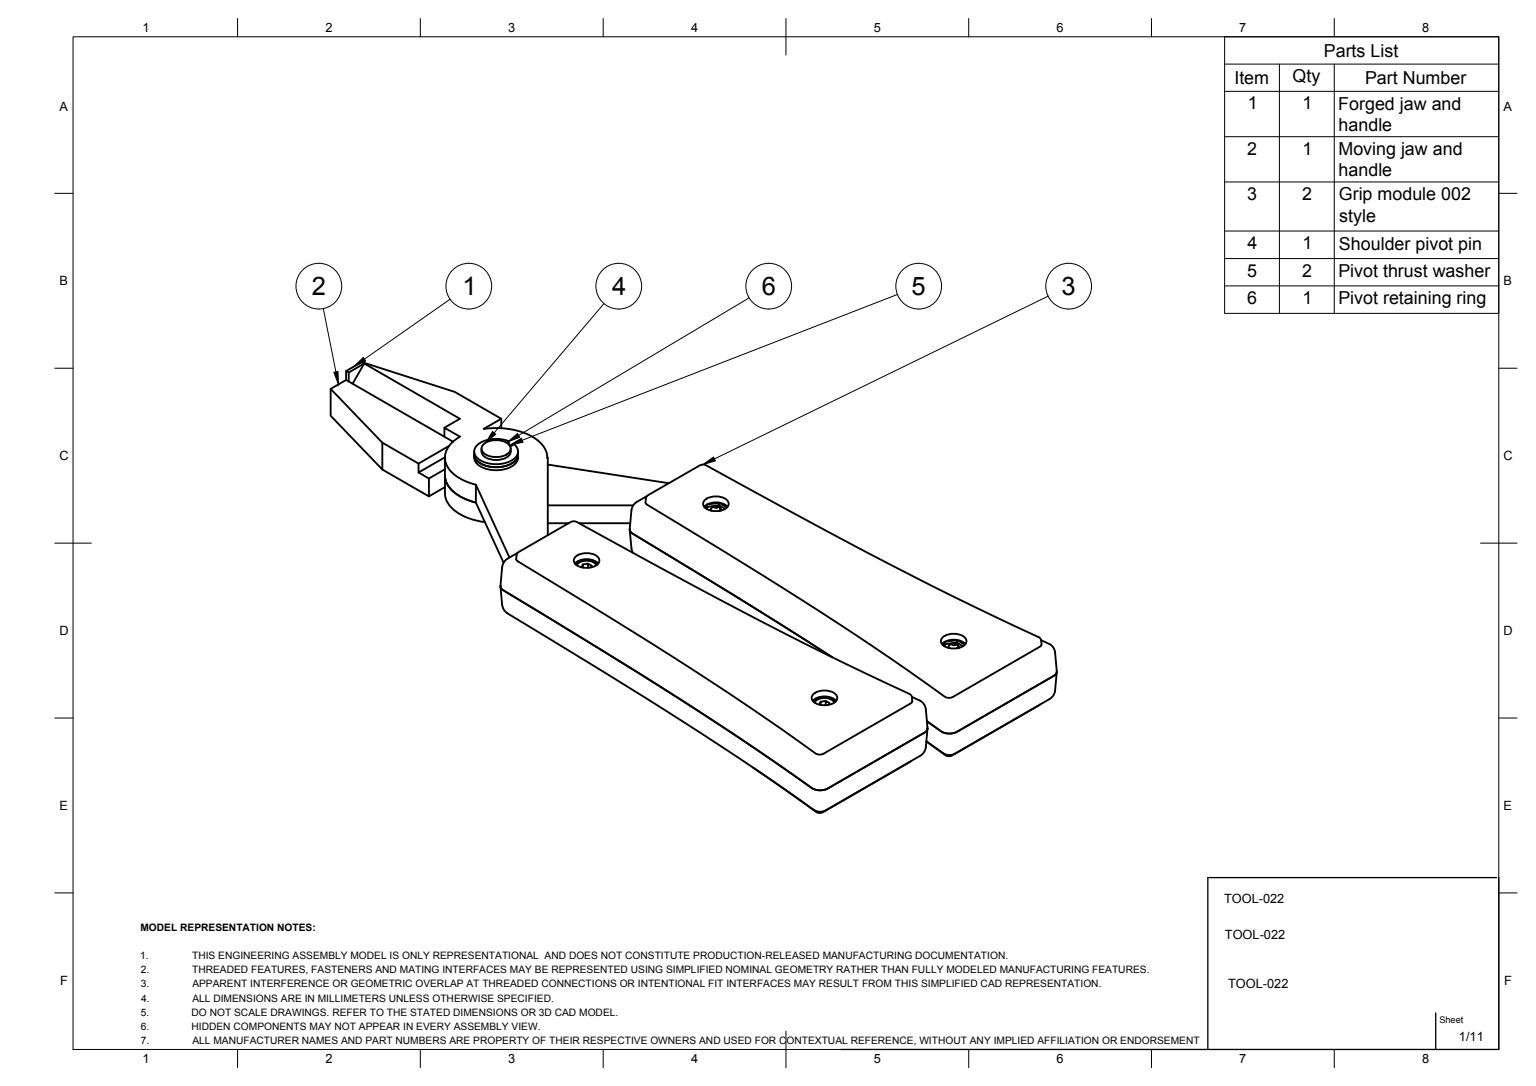
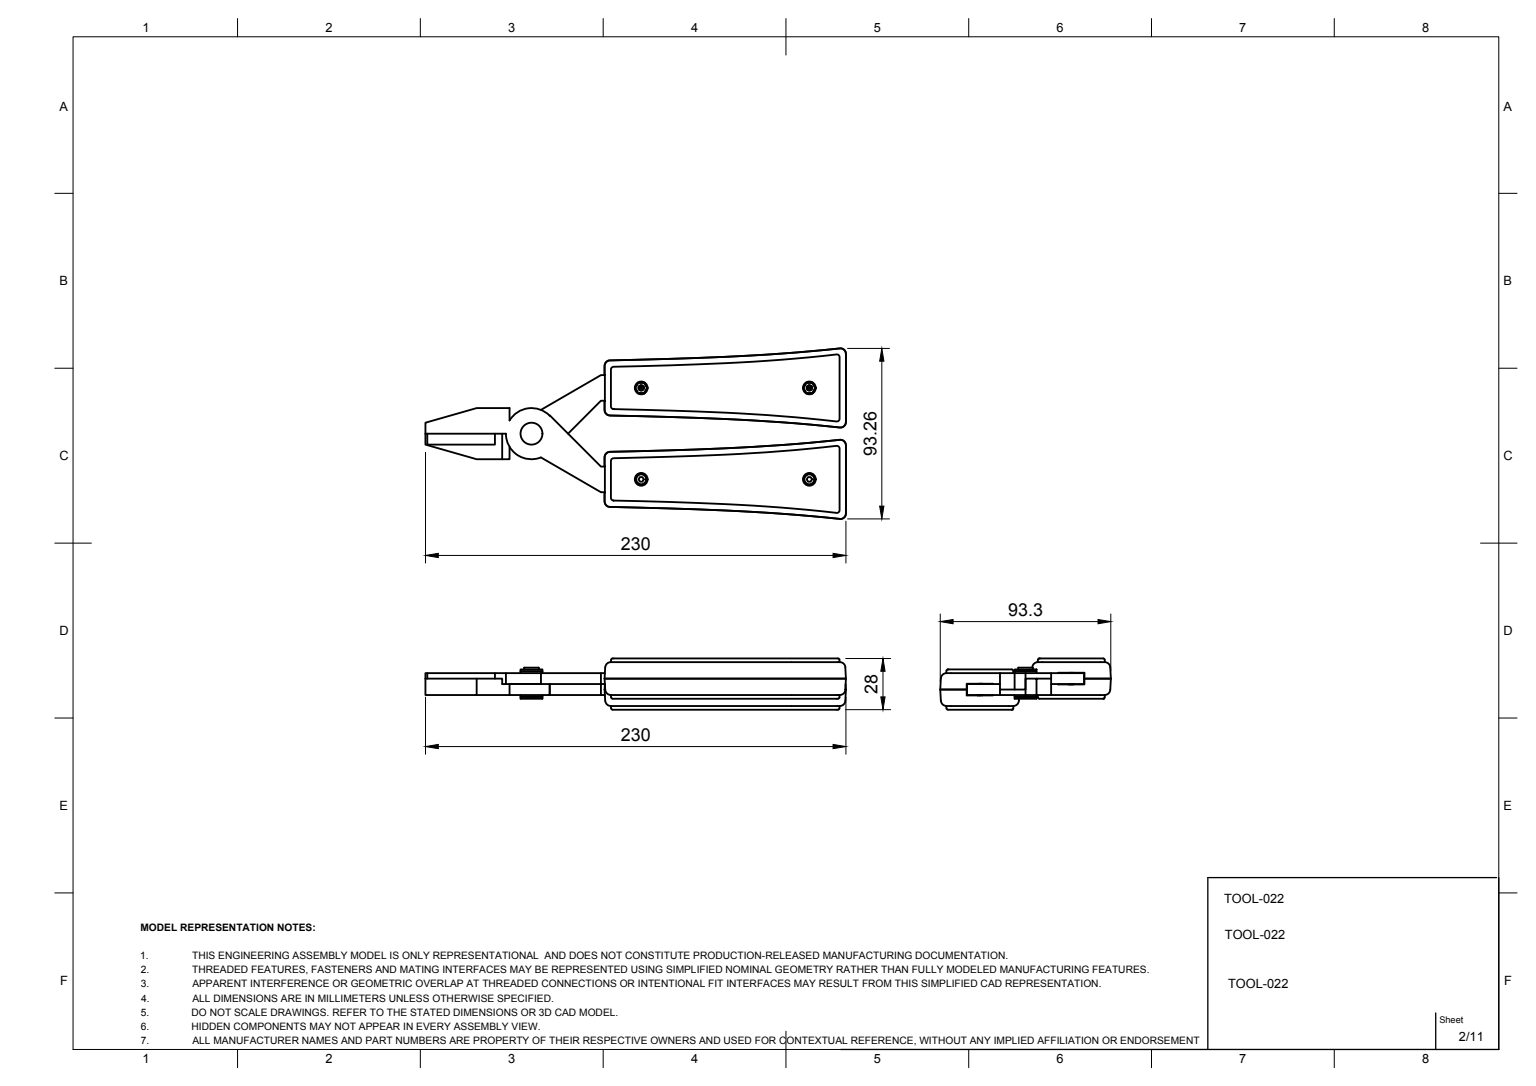
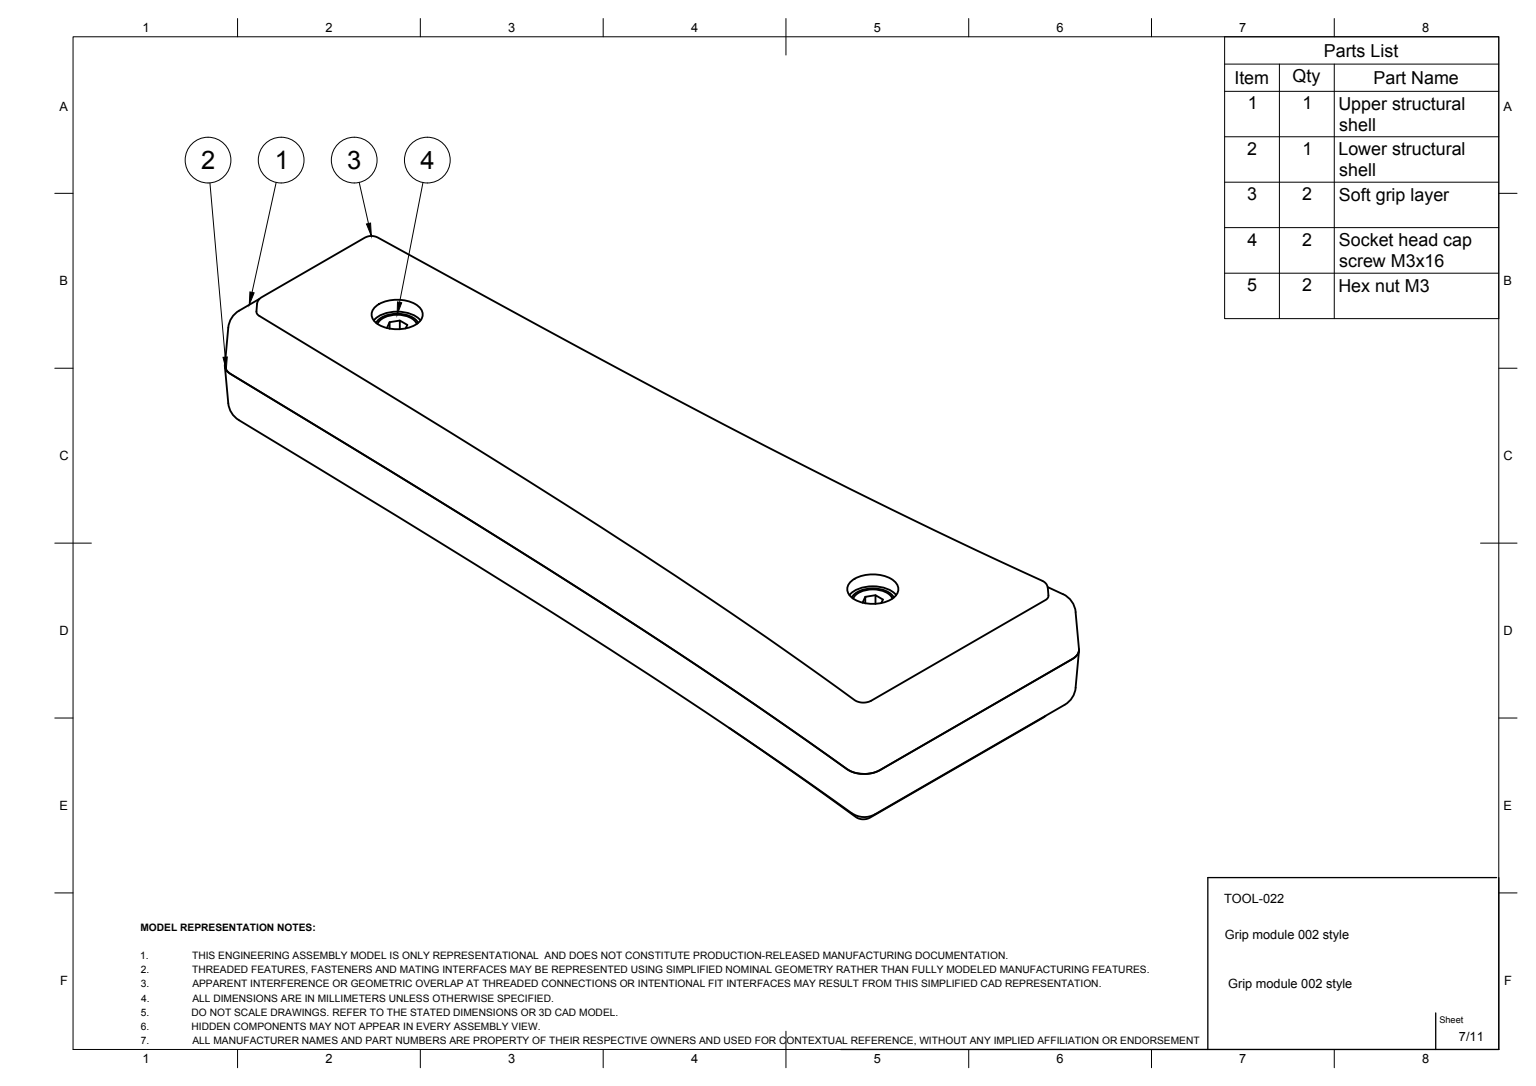
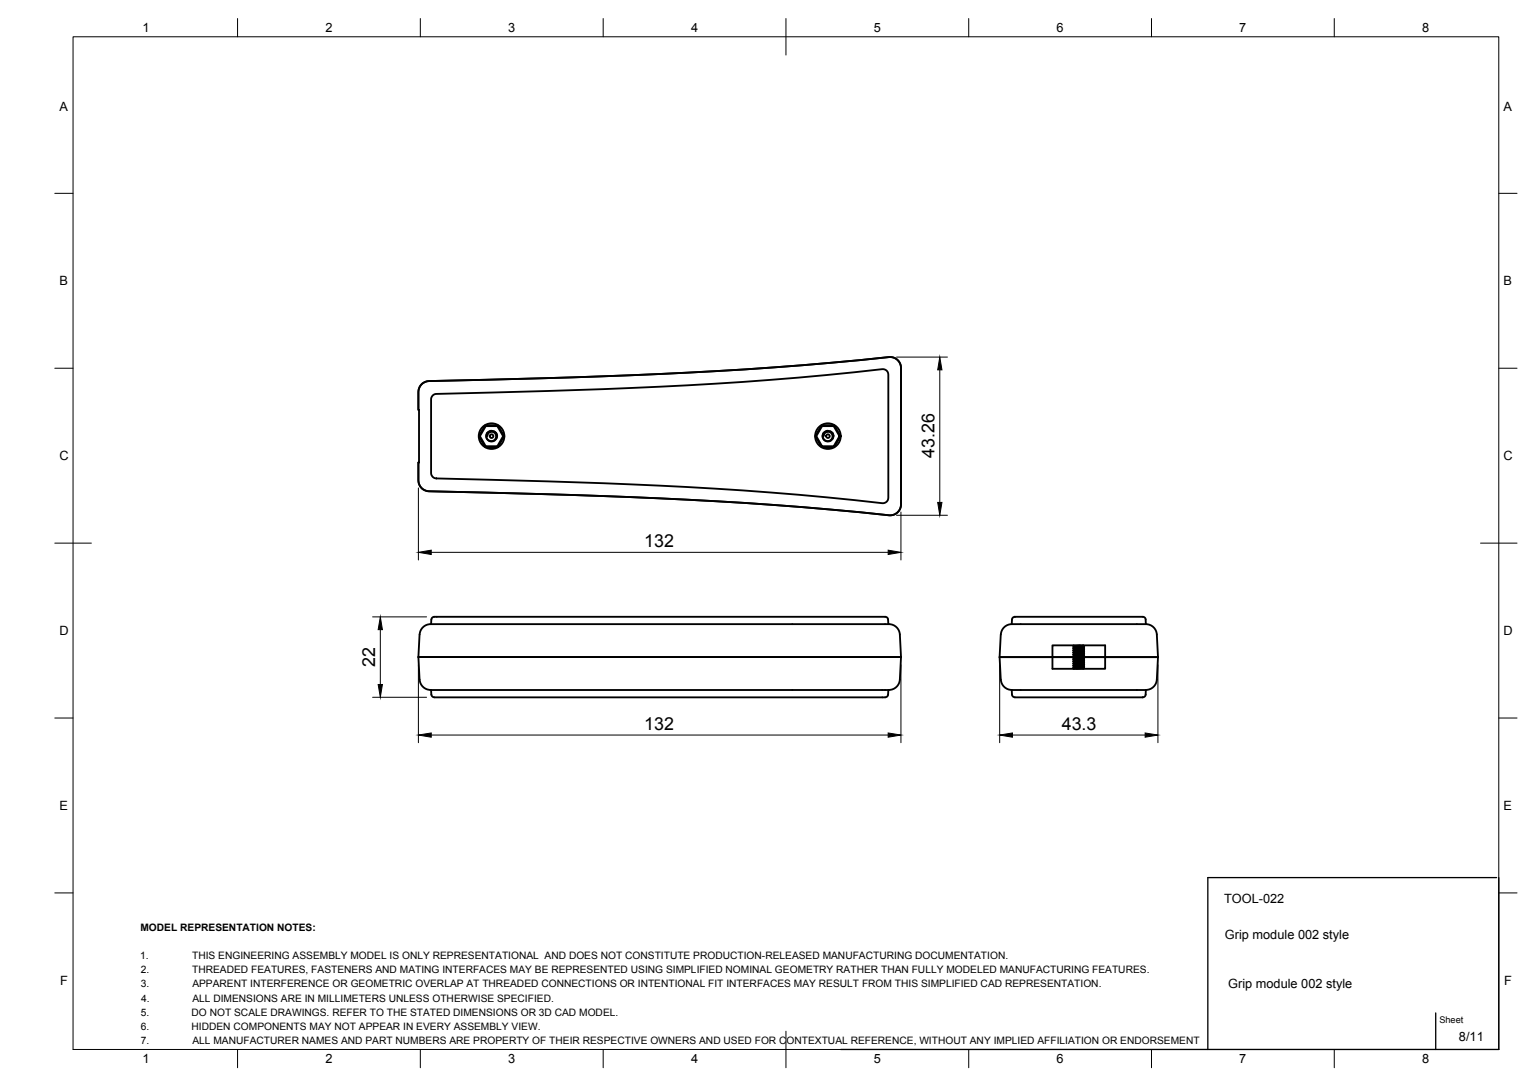
ISO-10303-21;
HEADER;
/* Generated by software containing ST-Developer
 * from STEP Tools, Inc. (www.steptools.com) 
 */

FILE_DESCRIPTION(
/* description */ (''),
/* implementation_level */ '2;1');

FILE_NAME(
/* name */ 'TOOL-022.step',
/* time_stamp */ '2026-11-10T08:27:36-08:00',
/* author */ (''),
/* organization */ (''),
/* preprocessor_version */ 'ST-DEVELOPER v20.2',
/* originating_system */ 'Autodesk Translation Framework v15.17.0.0',
/* authorisation */ '');

FILE_SCHEMA (('AUTOMOTIVE_DESIGN { 1 0 10303 214 3 1 1 }'));
ENDSEC;

DATA;
#10=MECHANICAL_DESIGN_GEOMETRIC_PRESENTATION_REPRESENTATION('',(#566,#567,
#568,#569,#570,#571,#572,#573,#574,#575),#19090);
#11=ITEM_DEFINED_TRANSFORMATION($,$,#7041,#7412);
#12=ITEM_DEFINED_TRANSFORMATION($,$,#7143,#7413);
#13=ITEM_DEFINED_TRANSFORMATION($,$,#7251,#7414);
#14=ITEM_DEFINED_TRANSFORMATION($,$,#7304,#7415);
#15=ITEM_DEFINED_TRANSFORMATION($,$,#7386,#7416);
#16=ITEM_DEFINED_TRANSFORMATION($,$,#7251,#7417);
#17=ITEM_DEFINED_TRANSFORMATION($,$,#7304,#7418);
#18=ITEM_DEFINED_TRANSFORMATION($,$,#7386,#7419);
#19=ITEM_DEFINED_TRANSFORMATION($,$,#6942,#7429);
#20=ITEM_DEFINED_TRANSFORMATION($,$,#6980,#7430);
#21=ITEM_DEFINED_TRANSFORMATION($,$,#7040,#7431);
#22=ITEM_DEFINED_TRANSFORMATION($,$,#7011,#7432);
#23=ITEM_DEFINED_TRANSFORMATION($,$,#7420,#7433);
#24=ITEM_DEFINED_TRANSFORMATION($,$,#7029,#7434);
#25=ITEM_DEFINED_TRANSFORMATION($,$,#7040,#7435);
#26=ITEM_DEFINED_TRANSFORMATION($,$,#7420,#7436);
#27=(
REPRESENTATION_RELATIONSHIP($,$,#19141,#19140)
REPRESENTATION_RELATIONSHIP_WITH_TRANSFORMATION(#11)
SHAPE_REPRESENTATION_RELATIONSHIP()
);
#28=(
REPRESENTATION_RELATIONSHIP($,$,#19142,#19140)
REPRESENTATION_RELATIONSHIP_WITH_TRANSFORMATION(#12)
SHAPE_REPRESENTATION_RELATIONSHIP()
);
#29=(
REPRESENTATION_RELATIONSHIP($,$,#19143,#19140)
REPRESENTATION_RELATIONSHIP_WITH_TRANSFORMATION(#13)
SHAPE_REPRESENTATION_RELATIONSHIP()
);
#30=(
REPRESENTATION_RELATIONSHIP($,$,#19144,#19140)
REPRESENTATION_RELATIONSHIP_WITH_TRANSFORMATION(#14)
SHAPE_REPRESENTATION_RELATIONSHIP()
);
#31=(
REPRESENTATION_RELATIONSHIP($,$,#19145,#19140)
REPRESENTATION_RELATIONSHIP_WITH_TRANSFORMATION(#15)
SHAPE_REPRESENTATION_RELATIONSHIP()
);
#32=(
REPRESENTATION_RELATIONSHIP($,$,#19143,#19140)
REPRESENTATION_RELATIONSHIP_WITH_TRANSFORMATION(#16)
SHAPE_REPRESENTATION_RELATIONSHIP()
);
#33=(
REPRESENTATION_RELATIONSHIP($,$,#19144,#19140)
REPRESENTATION_RELATIONSHIP_WITH_TRANSFORMATION(#17)
SHAPE_REPRESENTATION_RELATIONSHIP()
);
#34=(
REPRESENTATION_RELATIONSHIP($,$,#19145,#19140)
REPRESENTATION_RELATIONSHIP_WITH_TRANSFORMATION(#18)
SHAPE_REPRESENTATION_RELATIONSHIP()
);
#35=(
REPRESENTATION_RELATIONSHIP($,$,#19136,#19135)
REPRESENTATION_RELATIONSHIP_WITH_TRANSFORMATION(#19)
SHAPE_REPRESENTATION_RELATIONSHIP()
);
#36=(
REPRESENTATION_RELATIONSHIP($,$,#19137,#19135)
REPRESENTATION_RELATIONSHIP_WITH_TRANSFORMATION(#20)
SHAPE_REPRESENTATION_RELATIONSHIP()
);
#37=(
REPRESENTATION_RELATIONSHIP($,$,#19140,#19135)
REPRESENTATION_RELATIONSHIP_WITH_TRANSFORMATION(#21)
SHAPE_REPRESENTATION_RELATIONSHIP()
);
#38=(
REPRESENTATION_RELATIONSHIP($,$,#19138,#19135)
REPRESENTATION_RELATIONSHIP_WITH_TRANSFORMATION(#22)
SHAPE_REPRESENTATION_RELATIONSHIP()
);
#39=(
REPRESENTATION_RELATIONSHIP($,$,#19146,#19135)
REPRESENTATION_RELATIONSHIP_WITH_TRANSFORMATION(#23)
SHAPE_REPRESENTATION_RELATIONSHIP()
);
#40=(
REPRESENTATION_RELATIONSHIP($,$,#19139,#19135)
REPRESENTATION_RELATIONSHIP_WITH_TRANSFORMATION(#24)
SHAPE_REPRESENTATION_RELATIONSHIP()
);
#41=(
REPRESENTATION_RELATIONSHIP($,$,#19140,#19135)
REPRESENTATION_RELATIONSHIP_WITH_TRANSFORMATION(#25)
SHAPE_REPRESENTATION_RELATIONSHIP()
);
#42=(
REPRESENTATION_RELATIONSHIP($,$,#19146,#19135)
REPRESENTATION_RELATIONSHIP_WITH_TRANSFORMATION(#26)
SHAPE_REPRESENTATION_RELATIONSHIP()
);
#43=CONTEXT_DEPENDENT_SHAPE_REPRESENTATION(#27,#19118);
#44=CONTEXT_DEPENDENT_SHAPE_REPRESENTATION(#28,#19119);
#45=CONTEXT_DEPENDENT_SHAPE_REPRESENTATION(#29,#19120);
#46=CONTEXT_DEPENDENT_SHAPE_REPRESENTATION(#30,#19121);
#47=CONTEXT_DEPENDENT_SHAPE_REPRESENTATION(#31,#19122);
#48=CONTEXT_DEPENDENT_SHAPE_REPRESENTATION(#32,#19123);
#49=CONTEXT_DEPENDENT_SHAPE_REPRESENTATION(#33,#19124);
#50=CONTEXT_DEPENDENT_SHAPE_REPRESENTATION(#34,#19125);
#51=CONTEXT_DEPENDENT_SHAPE_REPRESENTATION(#35,#19127);
#52=CONTEXT_DEPENDENT_SHAPE_REPRESENTATION(#36,#19128);
#53=CONTEXT_DEPENDENT_SHAPE_REPRESENTATION(#37,#19129);
#54=CONTEXT_DEPENDENT_SHAPE_REPRESENTATION(#38,#19130);
#55=CONTEXT_DEPENDENT_SHAPE_REPRESENTATION(#39,#19131);
#56=CONTEXT_DEPENDENT_SHAPE_REPRESENTATION(#40,#19132);
#57=CONTEXT_DEPENDENT_SHAPE_REPRESENTATION(#41,#19133);
#58=CONTEXT_DEPENDENT_SHAPE_REPRESENTATION(#42,#19134);
#59=NEXT_ASSEMBLY_USAGE_OCCURRENCE('Upper structural shell:1',
'Upper structural shell:1','Upper structural shell:1',#19153,#19154,
'Upper structural shell:1');
#60=NEXT_ASSEMBLY_USAGE_OCCURRENCE('Lower structural shell:1',
'Lower structural shell:1','Lower structural shell:1',#19153,#19155,
'Lower structural shell:1');
#61=NEXT_ASSEMBLY_USAGE_OCCURRENCE('Soft grip layer:1',
'Soft grip layer:1','Soft grip layer:1',#19153,#19156,
'Soft grip layer:1');
#62=NEXT_ASSEMBLY_USAGE_OCCURRENCE('Socket head cap screw M3x16:1',
'Socket head cap screw M3x16:1','Socket head cap screw M3x16:1',#19153,
#19157,'Socket head cap screw M3x16:1');
#63=NEXT_ASSEMBLY_USAGE_OCCURRENCE('Hex nut M3:1','Hex nut M3:1',
'Hex nut M3:1',#19153,#19158,'Hex nut M3:1');
#64=NEXT_ASSEMBLY_USAGE_OCCURRENCE('Soft grip layer:2',
'Soft grip layer:2','Soft grip layer:2',#19153,#19156,
'Soft grip layer:2');
#65=NEXT_ASSEMBLY_USAGE_OCCURRENCE('Socket head cap screw M3x16:2',
'Socket head cap screw M3x16:2','Socket head cap screw M3x16:2',#19153,
#19157,'Socket head cap screw M3x16:2');
#66=NEXT_ASSEMBLY_USAGE_OCCURRENCE('Hex nut M3:2','Hex nut M3:2',
'Hex nut M3:2',#19153,#19158,'Hex nut M3:2');
#67=NEXT_ASSEMBLY_USAGE_OCCURRENCE('Forged jaw and handle:1',
'Forged jaw and handle:1','Forged jaw and handle:1',#19148,#19149,
'Forged jaw and handle:1');
#68=NEXT_ASSEMBLY_USAGE_OCCURRENCE('Moving jaw and handle:1',
'Moving jaw and handle:1','Moving jaw and handle:1',#19148,#19150,
'Moving jaw and handle:1');
#69=NEXT_ASSEMBLY_USAGE_OCCURRENCE('Grip module 002 style:1',
'Grip module 002 style:1','Grip module 002 style:1',#19148,#19153,
'Grip module 002 style:1');
#70=NEXT_ASSEMBLY_USAGE_OCCURRENCE('Shoulder pivot pin:1',
'Shoulder pivot pin:1','Shoulder pivot pin:1',#19148,#19151,
'Shoulder pivot pin:1');
#71=NEXT_ASSEMBLY_USAGE_OCCURRENCE('Pivot thrust washer:1',
'Pivot thrust washer:1','Pivot thrust washer:1',#19148,#19159,
'Pivot thrust washer:1');
#72=NEXT_ASSEMBLY_USAGE_OCCURRENCE('Pivot retaining ring:1',
'Pivot retaining ring:1','Pivot retaining ring:1',#19148,#19152,
'Pivot retaining ring:1');
#73=NEXT_ASSEMBLY_USAGE_OCCURRENCE('Grip module 002 style:2',
'Grip module 002 style:2','Grip module 002 style:2',#19148,#19153,
'Grip module 002 style:2');
#74=NEXT_ASSEMBLY_USAGE_OCCURRENCE('Pivot thrust washer:2',
'Pivot thrust washer:2','Pivot thrust washer:2',#19148,#19159,
'Pivot thrust washer:2');
#75=CONICAL_SURFACE('',#7367,0.1,0.785398163397448);
#76=SPHERICAL_SURFACE('',#7106,0.0999999999999999);
#77=SPHERICAL_SURFACE('',#7109,0.0999999999999997);
#78=SPHERICAL_SURFACE('',#7113,0.0999999999999998);
#79=SPHERICAL_SURFACE('',#7117,0.1);
#80=SPHERICAL_SURFACE('',#7122,0.3);
#81=SPHERICAL_SURFACE('',#7126,0.3);
#82=SPHERICAL_SURFACE('',#7130,0.3);
#83=SPHERICAL_SURFACE('',#7135,0.3);
#84=SPHERICAL_SURFACE('',#7214,0.0999999999999999);
#85=SPHERICAL_SURFACE('',#7217,0.0999999999999997);
#86=SPHERICAL_SURFACE('',#7221,0.0999999999999998);
#87=SPHERICAL_SURFACE('',#7225,0.1);
#88=SPHERICAL_SURFACE('',#7230,0.3);
#89=SPHERICAL_SURFACE('',#7234,0.3);
#90=SPHERICAL_SURFACE('',#7238,0.3);
#91=SPHERICAL_SURFACE('',#7243,0.3);
#92=B_SPLINE_SURFACE_WITH_KNOTS('',3,3,((#10183,#10184,#10185,#10186),(#10187,
#10188,#10189,#10190),(#10191,#10192,#10193,#10194),(#10195,#10196,#10197,
#10198)),.UNSPECIFIED.,.F.,.F.,.F.,(4,4),(4,4),(0.0600191787356395,0.326709122771036),
(0.0105314009467253,0.683686938235975),.UNSPECIFIED.);
#93=B_SPLINE_SURFACE_WITH_KNOTS('',3,3,((#10203,#10204,#10205,#10206),(#10207,
#10208,#10209,#10210),(#10211,#10212,#10213,#10214),(#10215,#10216,#10217,
#10218)),.UNSPECIFIED.,.F.,.F.,.F.,(4,4),(4,4),(0.0251675824878611,0.0470055662028096),
(0.0103663370325175,0.682341693918943),.UNSPECIFIED.);
#94=B_SPLINE_SURFACE_WITH_KNOTS('',3,3,((#10228,#10229,#10230,#10231),(#10232,
#10233,#10234,#10235),(#10236,#10237,#10238,#10239),(#10240,#10241,#10242,
#10243),(#10244,#10245,#10246,#10247)),.UNSPECIFIED.,.F.,.F.,.F.,(4,1,4),
(4,4),(0.,0.571428571428571,1.),(0.796205213256333,4.31873271634551),
 .UNSPECIFIED.);
#95=B_SPLINE_SURFACE_WITH_KNOTS('',3,3,((#10252,#10253,#10254,#10255),(#10256,
#10257,#10258,#10259),(#10260,#10261,#10262,#10263),(#10264,#10265,#10266,
#10267),(#10268,#10269,#10270,#10271)),.UNSPECIFIED.,.F.,.F.,.F.,(4,1,4),
(4,4),(0.,0.571428571428571,1.),(0.335767855111383,0.605460332260614),
 .UNSPECIFIED.);
#96=B_SPLINE_SURFACE_WITH_KNOTS('',3,3,((#10290,#10291,#10292,#10293),(#10294,
#10295,#10296,#10297),(#10298,#10299,#10300,#10301),(#10302,#10303,#10304,
#10305),(#10306,#10307,#10308,#10309)),.UNSPECIFIED.,.F.,.F.,.F.,(4,1,4),
(4,4),(0.,0.571428571428571,1.),(8.8675541747208,12.3900816778099),
 .UNSPECIFIED.);
#97=B_SPLINE_SURFACE_WITH_KNOTS('',3,3,((#10314,#10315,#10316,#10317),(#10318,
#10319,#10320,#10321),(#10322,#10323,#10324,#10325),(#10326,#10327,#10328,
#10329)),.UNSPECIFIED.,.F.,.F.,.F.,(4,4),(4,4),(0.673290877228964,0.939980821264432),
(0.010531400969624,0.683686938235975),.UNSPECIFIED.);
#98=B_SPLINE_SURFACE_WITH_KNOTS('',3,3,((#10330,#10331,#10332,#10333),(#10334,
#10335,#10336,#10337),(#10338,#10339,#10340,#10341),(#10342,#10343,#10344,
#10345)),.UNSPECIFIED.,.F.,.F.,.F.,(4,4),(4,4),(0.952994433797115,0.974832417512139),
(0.0103663370325174,0.682341693895801),.UNSPECIFIED.);
#99=B_SPLINE_SURFACE_WITH_KNOTS('',3,3,((#10429,#10430,#10431,#10432),(#10433,
#10434,#10435,#10436),(#10437,#10438,#10439,#10440),(#10441,#10442,#10443,
#10444)),.UNSPECIFIED.,.F.,.F.,.F.,(4,4),(4,4),(0.341076481775573,0.660379921919131),
(0.0113804342297301,0.684288445414502),.UNSPECIFIED.);
#100=B_SPLINE_SURFACE_WITH_KNOTS('',3,3,((#10449,#10450,#10451,#10452),
(#10453,#10454,#10455,#10456),(#10457,#10458,#10459,#10460),(#10461,#10462,
#10463,#10464),(#10465,#10466,#10467,#10468)),.UNSPECIFIED.,.F.,.F.,.F.,
(4,1,4),(4,4),(0.,0.571428571428571,1.),(4.5128966022766,8.72381854299666),
 .UNSPECIFIED.);
#101=B_SPLINE_SURFACE_WITH_KNOTS('',3,3,((#10478,#10479,#10480,#10481),
(#10482,#10483,#10484,#10485),(#10486,#10487,#10488,#10489),(#10490,#10491,
#10492,#10493),(#10494,#10495,#10496,#10497)),.UNSPECIFIED.,.F.,.F.,.F.,
(4,1,4),(4,4),(0.,0.571428571428571,1.),(4.46246834806959,8.67339028878965),
 .UNSPECIFIED.);
#102=B_SPLINE_SURFACE_WITH_KNOTS('',3,3,((#10502,#10503,#10504,#10505),
(#10506,#10507,#10508,#10509),(#10510,#10511,#10512,#10513),(#10514,#10515,
#10516,#10517)),.UNSPECIFIED.,.F.,.F.,.F.,(4,4),(4,4),(0.33962007808087,
0.658923518224427),(0.0113804342297301,0.68428844541339),.UNSPECIFIED.);
#103=B_SPLINE_SURFACE_WITH_KNOTS('',3,3,((#10589,#10590,#10591,#10592),
(#10593,#10594,#10595,#10596),(#10597,#10598,#10599,#10600),(#10601,#10602,
#10603,#10604)),.UNSPECIFIED.,.F.,.F.,.F.,(4,4),(4,4),(0.67474627241906,
0.91907102854965),(0.0117551961069005,0.684448842095107),.UNSPECIFIED.);
#104=B_SPLINE_SURFACE_WITH_KNOTS('',3,3,((#10609,#10610,#10611,#10612),
(#10613,#10614,#10615,#10616),(#10617,#10618,#10619,#10620),(#10621,#10622,
#10623,#10624),(#10625,#10626,#10627,#10628)),.UNSPECIFIED.,.F.,.F.,.F.,
(4,1,4),(4,4),(0.,0.571428571428571,1.),(8.92068531110742,12.1251256661408),
 .UNSPECIFIED.);
#105=B_SPLINE_SURFACE_WITH_KNOTS('',3,3,((#10629,#10630,#10631,#10632),
(#10633,#10634,#10635,#10636),(#10637,#10638,#10639,#10640),(#10641,#10642,
#10643,#10644),(#10645,#10646,#10647,#10648)),.UNSPECIFIED.,.F.,.F.,.F.,
(4,1,4),(4,4),(0.,0.571428571428571,1.),(1.06116122492545,4.26560157995882),
 .UNSPECIFIED.);
#106=B_SPLINE_SURFACE_WITH_KNOTS('',3,3,((#10653,#10654,#10655,#10656),
(#10657,#10658,#10659,#10660),(#10661,#10662,#10663,#10664),(#10665,#10666,
#10667,#10668)),.UNSPECIFIED.,.F.,.F.,.F.,(4,4),(4,4),(0.0809289714503497,
0.325253727580939),(0.011755196108102,0.684448842095106),.UNSPECIFIED.);
#107=B_SPLINE_SURFACE_WITH_KNOTS('',3,3,((#10743,#10744,#10745,#10746),
(#10747,#10748,#10749,#10750),(#10751,#10752,#10753,#10754),(#10755,#10756,
#10757,#10758)),.UNSPECIFIED.,.F.,.F.,.F.,(4,4),(4,4),(0.932204931312898,
0.977820042778932),(0.0118590921259657,0.68448768567755),.UNSPECIFIED.);
#108=B_SPLINE_SURFACE_WITH_KNOTS('',3,3,((#10768,#10769,#10770,#10771),
(#10772,#10773,#10774,#10775),(#10776,#10777,#10778,#10779),(#10780,#10781,
#10782,#10783),(#10784,#10785,#10786,#10787)),.UNSPECIFIED.,.F.,.F.,.F.,
(4,1,4),(4,4),(0.,0.571428571428571,1.),(12.3228618033436,12.893479658151),
 .UNSPECIFIED.);
#109=B_SPLINE_SURFACE_WITH_KNOTS('',3,3,((#10801,#10802,#10803,#10804),
(#10805,#10806,#10807,#10808),(#10809,#10810,#10811,#10812),(#10813,#10814,
#10815,#10816)),.UNSPECIFIED.,.F.,.F.,.F.,(4,4),(4,4),(0.0221799572210682,
0.0677950686870383),(0.0118590921467069,0.68448768567755),.UNSPECIFIED.);
#110=B_SPLINE_SURFACE_WITH_KNOTS('',3,3,((#10826,#10827,#10828,#10829),
(#10830,#10831,#10832,#10833),(#10834,#10835,#10836,#10837),(#10838,#10839,
#10840,#10841),(#10842,#10843,#10844,#10845)),.UNSPECIFIED.,.F.,.F.,.F.,
(4,1,4),(4,4),(0.,0.571428571428571,1.),(0.29280723291527,0.863425087722636),
 .UNSPECIFIED.);
#111=B_SPLINE_SURFACE_WITH_KNOTS('',3,3,((#10859,#10860,#10861,#10862),
(#10863,#10864,#10865,#10866),(#10867,#10868,#10869,#10870),(#10871,#10872,
#10873,#10874),(#10875,#10876,#10877,#10878)),.UNSPECIFIED.,.F.,.F.,.F.,
(4,1,4),(4,4),(0.,0.571428571428571,1.),(0.00866835330220971,0.617725317592517),
 .UNSPECIFIED.);
#112=B_SPLINE_SURFACE_WITH_KNOTS('',3,3,((#10885,#10886,#10887,#10888),
(#10889,#10890,#10891,#10892),(#10893,#10894,#10895,#10896),(#10897,#10898,
#10899,#10900),(#10901,#10902,#10903,#10904),(#10905,#10906,#10907,#10908)),
 .UNSPECIFIED.,.F.,.F.,.F.,(4,1,1,4),(4,4),(0.,0.285714285714286,0.571428571428571,
1.),(0.00654045782928703,0.615688454110788),.UNSPECIFIED.);
#113=B_SPLINE_SURFACE_WITH_KNOTS('',3,3,((#10913,#10914,#10915,#10916),
(#10917,#10918,#10919,#10920),(#10921,#10922,#10923,#10924),(#10925,#10926,
#10927,#10928),(#10929,#10930,#10931,#10932),(#10933,#10934,#10935,#10936)),
 .UNSPECIFIED.,.F.,.F.,.F.,(4,1,1,4),(4,4),(0.,0.285714285714286,0.571428571428571,
1.),(0.00659363931523289,0.615688454110787),.UNSPECIFIED.);
#114=B_SPLINE_SURFACE_WITH_KNOTS('',3,3,((#10941,#10942,#10943,#10944),
(#10945,#10946,#10947,#10948),(#10949,#10950,#10951,#10952),(#10953,#10954,
#10955,#10956),(#10957,#10958,#10959,#10960)),.UNSPECIFIED.,.F.,.F.,.F.,
(4,1,4),(4,4),(0.,0.571428571428571,1.),(12.5808265588057,12.8505190359549),
 .UNSPECIFIED.);
#115=B_SPLINE_SURFACE_WITH_KNOTS('',3,3,((#10961,#10962,#10963,#10964),
(#10965,#10966,#10967,#10968),(#10969,#10970,#10971,#10972),(#10973,#10974,
#10975,#10976),(#10977,#10978,#10979,#10980)),.UNSPECIFIED.,.F.,.F.,.F.,
(4,1,4),(4,4),(0.,0.571428571428571,1.),(0.00865878607617127,0.617725317592517),
 .UNSPECIFIED.);
#116=B_SPLINE_SURFACE_WITH_KNOTS('',3,3,((#11006,#11007,#11008,#11009),
(#11010,#11011,#11012,#11013),(#11014,#11015,#11016,#11017),(#11018,#11019,
#11020,#11021),(#11022,#11023,#11024,#11025)),.UNSPECIFIED.,.F.,.F.,.F.,
(4,1,4),(4,4),(0.,0.571428571428571,1.),(-0.00615755989250974,0.617725317592517),
 .UNSPECIFIED.);
#117=B_SPLINE_SURFACE_WITH_KNOTS('',3,3,((#11044,#11045,#11046,#11047,#11048),
(#11049,#11050,#11051,#11052,#11053),(#11054,#11055,#11056,#11057,#11058),
(#11059,#11060,#11061,#11062,#11063),(#11064,#11065,#11066,#11067,#11068)),
 .UNSPECIFIED.,.F.,.F.,.F.,(4,1,4),(4,1,4),(0.,0.571428571428571,1.),(0.335767855111383,
5.71764434212835,12.893479658151),.UNSPECIFIED.);
#118=B_SPLINE_SURFACE_WITH_KNOTS('',3,3,((#11079,#11080,#11081,#11082),
(#11083,#11084,#11085,#11086),(#11087,#11088,#11089,#11090),(#11091,#11092,
#11093,#11094),(#11095,#11096,#11097,#11098),(#11099,#11100,#11101,#11102)),
 .UNSPECIFIED.,.F.,.F.,.F.,(4,1,1,4),(4,4),(0.,0.285714285714286,0.571428571428571,
1.),(-0.00844595120920508,0.615688454110788),.UNSPECIFIED.);
#119=B_SPLINE_SURFACE_WITH_KNOTS('',3,3,((#11111,#11112,#11113,#11114),
(#11115,#11116,#11117,#11118),(#11119,#11120,#11121,#11122),(#11123,#11124,
#11125,#11126),(#11127,#11128,#11129,#11130),(#11131,#11132,#11133,#11134)),
 .UNSPECIFIED.,.F.,.F.,.F.,(4,1,1,4),(4,4),(0.,0.285714285714286,0.571428571428571,
1.),(-0.00828643285111643,0.615688454110787),.UNSPECIFIED.);
#120=B_SPLINE_SURFACE_WITH_KNOTS('',3,3,((#11143,#11144,#11145,#11146,#11147),
(#11148,#11149,#11150,#11151,#11152),(#11153,#11154,#11155,#11156,#11157),
(#11158,#11159,#11160,#11161,#11162),(#11163,#11164,#11165,#11166,#11167)),
 .UNSPECIFIED.,.F.,.F.,.F.,(4,1,4),(4,1,4),(0.,0.571428571428571,1.),(0.29280723291527,
7.4686425489379,12.8505190359549),.UNSPECIFIED.);
#121=B_SPLINE_SURFACE_WITH_KNOTS('',3,3,((#11178,#11179,#11180,#11181),
(#11182,#11183,#11184,#11185),(#11186,#11187,#11188,#11189),(#11190,#11191,
#11192,#11193),(#11194,#11195,#11196,#11197)),.UNSPECIFIED.,.F.,.F.,.F.,
(4,1,4),(4,4),(0.,0.571428571428571,1.),(-0.0061862132014275,0.617725317592517),
 .UNSPECIFIED.);
#122=B_SPLINE_SURFACE_WITH_KNOTS('',3,3,((#11206,#11207,#11208,#11209),
(#11210,#11211,#11212,#11213),(#11214,#11215,#11216,#11217),(#11218,#11219,
#11220,#11221)),.UNSPECIFIED.,.F.,.F.,.F.,(4,4),(4,4),(0.025165545222094,
0.977821881680028),(0.,0.68448768567755),.UNSPECIFIED.);
#123=B_SPLINE_SURFACE_WITH_KNOTS('',3,3,((#11224,#11225,#11226,#11227),
(#11228,#11229,#11230,#11231),(#11232,#11233,#11234,#11235),(#11236,#11237,
#11238,#11239)),.UNSPECIFIED.,.F.,.F.,.F.,(4,4),(4,4),(0.0221781183199723,
0.974834454777906),(0.,0.68448768567755),.UNSPECIFIED.);
#124=B_SPLINE_SURFACE_WITH_KNOTS('',3,3,((#12291,#12292,#12293,#12294),
(#12295,#12296,#12297,#12298),(#12299,#12300,#12301,#12302),(#12303,#12304,
#12305,#12306)),.UNSPECIFIED.,.F.,.F.,.F.,(4,4),(4,4),(0.0600191787356395,
0.326709122771036),(0.0105314009467253,0.683686938235975),.UNSPECIFIED.);
#125=B_SPLINE_SURFACE_WITH_KNOTS('',3,3,((#12311,#12312,#12313,#12314),
(#12315,#12316,#12317,#12318),(#12319,#12320,#12321,#12322),(#12323,#12324,
#12325,#12326)),.UNSPECIFIED.,.F.,.F.,.F.,(4,4),(4,4),(0.0251675824878611,
0.0470055662028096),(0.0103663370325175,0.682341693918943),
 .UNSPECIFIED.);
#126=B_SPLINE_SURFACE_WITH_KNOTS('',3,3,((#12336,#12337,#12338,#12339),
(#12340,#12341,#12342,#12343),(#12344,#12345,#12346,#12347),(#12348,#12349,
#12350,#12351),(#12352,#12353,#12354,#12355)),.UNSPECIFIED.,.F.,.F.,.F.,
(4,1,4),(4,4),(0.,0.571428571428571,1.),(0.796205213256333,4.31873271634551),
 .UNSPECIFIED.);
#127=B_SPLINE_SURFACE_WITH_KNOTS('',3,3,((#12360,#12361,#12362,#12363),
(#12364,#12365,#12366,#12367),(#12368,#12369,#12370,#12371),(#12372,#12373,
#12374,#12375),(#12376,#12377,#12378,#12379)),.UNSPECIFIED.,.F.,.F.,.F.,
(4,1,4),(4,4),(0.,0.571428571428571,1.),(0.335767855111383,0.605460332260614),
 .UNSPECIFIED.);
#128=B_SPLINE_SURFACE_WITH_KNOTS('',3,3,((#12398,#12399,#12400,#12401),
(#12402,#12403,#12404,#12405),(#12406,#12407,#12408,#12409),(#12410,#12411,
#12412,#12413),(#12414,#12415,#12416,#12417)),.UNSPECIFIED.,.F.,.F.,.F.,
(4,1,4),(4,4),(0.,0.571428571428571,1.),(8.8675541747208,12.3900816778099),
 .UNSPECIFIED.);
#129=B_SPLINE_SURFACE_WITH_KNOTS('',3,3,((#12422,#12423,#12424,#12425),
(#12426,#12427,#12428,#12429),(#12430,#12431,#12432,#12433),(#12434,#12435,
#12436,#12437)),.UNSPECIFIED.,.F.,.F.,.F.,(4,4),(4,4),(0.673290877228964,
0.939980821264432),(0.010531400969624,0.683686938235975),.UNSPECIFIED.);
#130=B_SPLINE_SURFACE_WITH_KNOTS('',3,3,((#12438,#12439,#12440,#12441),
(#12442,#12443,#12444,#12445),(#12446,#12447,#12448,#12449),(#12450,#12451,
#12452,#12453)),.UNSPECIFIED.,.F.,.F.,.F.,(4,4),(4,4),(0.952994433797115,
0.974832417512139),(0.0103663370325174,0.682341693895801),.UNSPECIFIED.);
#131=B_SPLINE_SURFACE_WITH_KNOTS('',3,3,((#12537,#12538,#12539,#12540),
(#12541,#12542,#12543,#12544),(#12545,#12546,#12547,#12548),(#12549,#12550,
#12551,#12552)),.UNSPECIFIED.,.F.,.F.,.F.,(4,4),(4,4),(0.341076481775573,
0.660379921919131),(0.0113804342297301,0.684288445414502),.UNSPECIFIED.);
#132=B_SPLINE_SURFACE_WITH_KNOTS('',3,3,((#12557,#12558,#12559,#12560),
(#12561,#12562,#12563,#12564),(#12565,#12566,#12567,#12568),(#12569,#12570,
#12571,#12572),(#12573,#12574,#12575,#12576)),.UNSPECIFIED.,.F.,.F.,.F.,
(4,1,4),(4,4),(0.,0.571428571428571,1.),(4.5128966022766,8.72381854299666),
 .UNSPECIFIED.);
#133=B_SPLINE_SURFACE_WITH_KNOTS('',3,3,((#12586,#12587,#12588,#12589),
(#12590,#12591,#12592,#12593),(#12594,#12595,#12596,#12597),(#12598,#12599,
#12600,#12601),(#12602,#12603,#12604,#12605)),.UNSPECIFIED.,.F.,.F.,.F.,
(4,1,4),(4,4),(0.,0.571428571428571,1.),(4.46246834806959,8.67339028878965),
 .UNSPECIFIED.);
#134=B_SPLINE_SURFACE_WITH_KNOTS('',3,3,((#12610,#12611,#12612,#12613),
(#12614,#12615,#12616,#12617),(#12618,#12619,#12620,#12621),(#12622,#12623,
#12624,#12625)),.UNSPECIFIED.,.F.,.F.,.F.,(4,4),(4,4),(0.33962007808087,
0.658923518224427),(0.0113804342297301,0.68428844541339),.UNSPECIFIED.);
#135=B_SPLINE_SURFACE_WITH_KNOTS('',3,3,((#12697,#12698,#12699,#12700),
(#12701,#12702,#12703,#12704),(#12705,#12706,#12707,#12708),(#12709,#12710,
#12711,#12712)),.UNSPECIFIED.,.F.,.F.,.F.,(4,4),(4,4),(0.67474627241906,
0.91907102854965),(0.0117551961069005,0.684448842095107),.UNSPECIFIED.);
#136=B_SPLINE_SURFACE_WITH_KNOTS('',3,3,((#12717,#12718,#12719,#12720),
(#12721,#12722,#12723,#12724),(#12725,#12726,#12727,#12728),(#12729,#12730,
#12731,#12732),(#12733,#12734,#12735,#12736)),.UNSPECIFIED.,.F.,.F.,.F.,
(4,1,4),(4,4),(0.,0.571428571428571,1.),(8.92068531110742,12.1251256661408),
 .UNSPECIFIED.);
#137=B_SPLINE_SURFACE_WITH_KNOTS('',3,3,((#12737,#12738,#12739,#12740),
(#12741,#12742,#12743,#12744),(#12745,#12746,#12747,#12748),(#12749,#12750,
#12751,#12752),(#12753,#12754,#12755,#12756)),.UNSPECIFIED.,.F.,.F.,.F.,
(4,1,4),(4,4),(0.,0.571428571428571,1.),(1.06116122492545,4.26560157995882),
 .UNSPECIFIED.);
#138=B_SPLINE_SURFACE_WITH_KNOTS('',3,3,((#12761,#12762,#12763,#12764),
(#12765,#12766,#12767,#12768),(#12769,#12770,#12771,#12772),(#12773,#12774,
#12775,#12776)),.UNSPECIFIED.,.F.,.F.,.F.,(4,4),(4,4),(0.0809289714503497,
0.325253727580939),(0.011755196108102,0.684448842095106),.UNSPECIFIED.);
#139=B_SPLINE_SURFACE_WITH_KNOTS('',3,3,((#12851,#12852,#12853,#12854),
(#12855,#12856,#12857,#12858),(#12859,#12860,#12861,#12862),(#12863,#12864,
#12865,#12866)),.UNSPECIFIED.,.F.,.F.,.F.,(4,4),(4,4),(0.932204931312898,
0.977820042778932),(0.0118590921259657,0.68448768567755),.UNSPECIFIED.);
#140=B_SPLINE_SURFACE_WITH_KNOTS('',3,3,((#12876,#12877,#12878,#12879),
(#12880,#12881,#12882,#12883),(#12884,#12885,#12886,#12887),(#12888,#12889,
#12890,#12891),(#12892,#12893,#12894,#12895)),.UNSPECIFIED.,.F.,.F.,.F.,
(4,1,4),(4,4),(0.,0.571428571428571,1.),(12.3228618033436,12.893479658151),
 .UNSPECIFIED.);
#141=B_SPLINE_SURFACE_WITH_KNOTS('',3,3,((#12909,#12910,#12911,#12912),
(#12913,#12914,#12915,#12916),(#12917,#12918,#12919,#12920),(#12921,#12922,
#12923,#12924)),.UNSPECIFIED.,.F.,.F.,.F.,(4,4),(4,4),(0.0221799572210682,
0.0677950686870383),(0.0118590921467069,0.68448768567755),.UNSPECIFIED.);
#142=B_SPLINE_SURFACE_WITH_KNOTS('',3,3,((#12934,#12935,#12936,#12937),
(#12938,#12939,#12940,#12941),(#12942,#12943,#12944,#12945),(#12946,#12947,
#12948,#12949),(#12950,#12951,#12952,#12953)),.UNSPECIFIED.,.F.,.F.,.F.,
(4,1,4),(4,4),(0.,0.571428571428571,1.),(0.29280723291527,0.863425087722636),
 .UNSPECIFIED.);
#143=B_SPLINE_SURFACE_WITH_KNOTS('',3,3,((#12967,#12968,#12969,#12970),
(#12971,#12972,#12973,#12974),(#12975,#12976,#12977,#12978),(#12979,#12980,
#12981,#12982),(#12983,#12984,#12985,#12986)),.UNSPECIFIED.,.F.,.F.,.F.,
(4,1,4),(4,4),(0.,0.571428571428571,1.),(0.00866835330220971,0.617725317592517),
 .UNSPECIFIED.);
#144=B_SPLINE_SURFACE_WITH_KNOTS('',3,3,((#12993,#12994,#12995,#12996),
(#12997,#12998,#12999,#13000),(#13001,#13002,#13003,#13004),(#13005,#13006,
#13007,#13008),(#13009,#13010,#13011,#13012),(#13013,#13014,#13015,#13016)),
 .UNSPECIFIED.,.F.,.F.,.F.,(4,1,1,4),(4,4),(0.,0.285714285714286,0.571428571428571,
1.),(0.00654045782928703,0.615688454110788),.UNSPECIFIED.);
#145=B_SPLINE_SURFACE_WITH_KNOTS('',3,3,((#13021,#13022,#13023,#13024),
(#13025,#13026,#13027,#13028),(#13029,#13030,#13031,#13032),(#13033,#13034,
#13035,#13036),(#13037,#13038,#13039,#13040),(#13041,#13042,#13043,#13044)),
 .UNSPECIFIED.,.F.,.F.,.F.,(4,1,1,4),(4,4),(0.,0.285714285714286,0.571428571428571,
1.),(0.00659363931523289,0.615688454110787),.UNSPECIFIED.);
#146=B_SPLINE_SURFACE_WITH_KNOTS('',3,3,((#13049,#13050,#13051,#13052),
(#13053,#13054,#13055,#13056),(#13057,#13058,#13059,#13060),(#13061,#13062,
#13063,#13064),(#13065,#13066,#13067,#13068)),.UNSPECIFIED.,.F.,.F.,.F.,
(4,1,4),(4,4),(0.,0.571428571428571,1.),(12.5808265588057,12.8505190359549),
 .UNSPECIFIED.);
#147=B_SPLINE_SURFACE_WITH_KNOTS('',3,3,((#13069,#13070,#13071,#13072),
(#13073,#13074,#13075,#13076),(#13077,#13078,#13079,#13080),(#13081,#13082,
#13083,#13084),(#13085,#13086,#13087,#13088)),.UNSPECIFIED.,.F.,.F.,.F.,
(4,1,4),(4,4),(0.,0.571428571428571,1.),(0.00865878607617127,0.617725317592517),
 .UNSPECIFIED.);
#148=B_SPLINE_SURFACE_WITH_KNOTS('',3,3,((#13114,#13115,#13116,#13117),
(#13118,#13119,#13120,#13121),(#13122,#13123,#13124,#13125),(#13126,#13127,
#13128,#13129),(#13130,#13131,#13132,#13133)),.UNSPECIFIED.,.F.,.F.,.F.,
(4,1,4),(4,4),(0.,0.571428571428571,1.),(-0.00615755989250974,0.617725317592517),
 .UNSPECIFIED.);
#149=B_SPLINE_SURFACE_WITH_KNOTS('',3,3,((#13152,#13153,#13154,#13155,#13156),
(#13157,#13158,#13159,#13160,#13161),(#13162,#13163,#13164,#13165,#13166),
(#13167,#13168,#13169,#13170,#13171),(#13172,#13173,#13174,#13175,#13176)),
 .UNSPECIFIED.,.F.,.F.,.F.,(4,1,4),(4,1,4),(0.,0.571428571428571,1.),(0.335767855111383,
5.71764434212835,12.893479658151),.UNSPECIFIED.);
#150=B_SPLINE_SURFACE_WITH_KNOTS('',3,3,((#13187,#13188,#13189,#13190),
(#13191,#13192,#13193,#13194),(#13195,#13196,#13197,#13198),(#13199,#13200,
#13201,#13202),(#13203,#13204,#13205,#13206),(#13207,#13208,#13209,#13210)),
 .UNSPECIFIED.,.F.,.F.,.F.,(4,1,1,4),(4,4),(0.,0.285714285714286,0.571428571428571,
1.),(-0.00844595120920508,0.615688454110788),.UNSPECIFIED.);
#151=B_SPLINE_SURFACE_WITH_KNOTS('',3,3,((#13219,#13220,#13221,#13222),
(#13223,#13224,#13225,#13226),(#13227,#13228,#13229,#13230),(#13231,#13232,
#13233,#13234),(#13235,#13236,#13237,#13238),(#13239,#13240,#13241,#13242)),
 .UNSPECIFIED.,.F.,.F.,.F.,(4,1,1,4),(4,4),(0.,0.285714285714286,0.571428571428571,
1.),(-0.00828643285111643,0.615688454110787),.UNSPECIFIED.);
#152=B_SPLINE_SURFACE_WITH_KNOTS('',3,3,((#13251,#13252,#13253,#13254,#13255),
(#13256,#13257,#13258,#13259,#13260),(#13261,#13262,#13263,#13264,#13265),
(#13266,#13267,#13268,#13269,#13270),(#13271,#13272,#13273,#13274,#13275)),
 .UNSPECIFIED.,.F.,.F.,.F.,(4,1,4),(4,1,4),(0.,0.571428571428571,1.),(0.29280723291527,
7.4686425489379,12.8505190359549),.UNSPECIFIED.);
#153=B_SPLINE_SURFACE_WITH_KNOTS('',3,3,((#13286,#13287,#13288,#13289),
(#13290,#13291,#13292,#13293),(#13294,#13295,#13296,#13297),(#13298,#13299,
#13300,#13301),(#13302,#13303,#13304,#13305)),.UNSPECIFIED.,.F.,.F.,.F.,
(4,1,4),(4,4),(0.,0.571428571428571,1.),(-0.0061862132014275,0.617725317592517),
 .UNSPECIFIED.);
#154=B_SPLINE_SURFACE_WITH_KNOTS('',3,3,((#13314,#13315,#13316,#13317),
(#13318,#13319,#13320,#13321),(#13322,#13323,#13324,#13325),(#13326,#13327,
#13328,#13329)),.UNSPECIFIED.,.F.,.F.,.F.,(4,4),(4,4),(0.025165545222094,
0.977821881680028),(0.,0.68448768567755),.UNSPECIFIED.);
#155=B_SPLINE_SURFACE_WITH_KNOTS('',3,3,((#13332,#13333,#13334,#13335),
(#13336,#13337,#13338,#13339),(#13340,#13341,#13342,#13343),(#13344,#13345,
#13346,#13347)),.UNSPECIFIED.,.F.,.F.,.F.,(4,4),(4,4),(0.0221781183199723,
0.974834454777906),(0.,0.68448768567755),.UNSPECIFIED.);
#156=B_SPLINE_SURFACE_WITH_KNOTS('',3,3,((#13418,#13419,#13420,#13421,#13422),
(#13423,#13424,#13425,#13426,#13427),(#13428,#13429,#13430,#13431,#13432),
(#13433,#13434,#13435,#13436,#13437),(#13438,#13439,#13440,#13441,#13442)),
 .UNSPECIFIED.,.F.,.F.,.F.,(4,1,4),(4,1,4),(0.,0.571428571428571,1.),(0.,
0.0505788685273923,0.118017359897249),.UNSPECIFIED.);
#157=B_SPLINE_SURFACE_WITH_KNOTS('',3,3,((#13465,#13466,#13467,#13468,#13469),
(#13470,#13471,#13472,#13473,#13474),(#13475,#13476,#13477,#13478,#13479),
(#13480,#13481,#13482,#13483,#13484),(#13485,#13486,#13487,#13488,#13489)),
 .UNSPECIFIED.,.F.,.F.,.F.,(4,1,4),(4,1,4),(0.,0.571428571428571,1.),(0.,
0.0505788685278266,0.118017359898262),.UNSPECIFIED.);
#158=B_SPLINE_SURFACE_WITH_KNOTS('',3,3,((#13503,#13504,#13505,#13506,#13507),
(#13508,#13509,#13510,#13511,#13512),(#13513,#13514,#13515,#13516,#13517),
(#13518,#13519,#13520,#13521,#13522),(#13523,#13524,#13525,#13526,#13527)),
 .UNSPECIFIED.,.F.,.F.,.F.,(4,1,4),(4,1,4),(0.,0.571428571428571,1.),(0.,
5.23288834931112,12.2100728150593),.UNSPECIFIED.);
#159=B_SPLINE_SURFACE_WITH_KNOTS('',3,3,((#13541,#13542,#13543,#13544,#13545),
(#13546,#13547,#13548,#13549,#13550),(#13551,#13552,#13553,#13554,#13555),
(#13556,#13557,#13558,#13559,#13560),(#13561,#13562,#13563,#13564,#13565)),
 .UNSPECIFIED.,.F.,.F.,.F.,(4,1,4),(4,1,4),(0.,0.571428571428571,1.),(1.97133828064127E-11,
0.0463413823988794,0.108129892237767),.UNSPECIFIED.);
#160=B_SPLINE_SURFACE_WITH_KNOTS('',3,3,((#13585,#13586,#13587,#13588,#13589),
(#13590,#13591,#13592,#13593,#13594),(#13595,#13596,#13597,#13598,#13599),
(#13600,#13601,#13602,#13603,#13604),(#13605,#13606,#13607,#13608,#13609)),
 .UNSPECIFIED.,.F.,.F.,.F.,(4,1,4),(4,1,4),(0.,0.571428571428571,1.),(0.,
0.0463413823743492,0.108129892206815),.UNSPECIFIED.);
#161=B_SPLINE_SURFACE_WITH_KNOTS('',3,3,((#13623,#13624,#13625,#13626,#13627),
(#13628,#13629,#13630,#13631,#13632),(#13633,#13634,#13635,#13636,#13637),
(#13638,#13639,#13640,#13641,#13642),(#13643,#13644,#13645,#13646,#13647)),
 .UNSPECIFIED.,.F.,.F.,.F.,(4,1,4),(4,1,4),(0.,0.571428571428571,1.),(6.51086303075479E-13,
6.97718480957529,12.2100734167563),.UNSPECIFIED.);
#162=B_SPLINE_SURFACE_WITH_KNOTS('',3,3,((#13670,#13671,#13672,#13673),
(#13674,#13675,#13676,#13677),(#13678,#13679,#13680,#13681),(#13682,#13683,
#13684,#13685),(#13686,#13687,#13688,#13689)),.UNSPECIFIED.,.F.,.F.,.F.,
(4,1,4),(4,4),(0.,0.571428571428571,1.),(-0.00308447593286339,0.124708996845866),
 .UNSPECIFIED.);
#163=B_SPLINE_SURFACE_WITH_KNOTS('',3,3,((#13723,#13724,#13725,#13726),
(#13727,#13728,#13729,#13730),(#13731,#13732,#13733,#13734),(#13735,#13736,
#13737,#13738)),.UNSPECIFIED.,.F.,.F.,.F.,(4,4),(4,4),(0.0116899650356219,
0.986620910196183),(0.,0.621418053543664),.UNSPECIFIED.);
#164=B_SPLINE_SURFACE_WITH_KNOTS('',3,3,((#13748,#13749,#13750,#13751),
(#13752,#13753,#13754,#13755),(#13756,#13757,#13758,#13759),(#13760,#13761,
#13762,#13763),(#13764,#13765,#13766,#13767),(#13768,#13769,#13770,#13771)),
 .UNSPECIFIED.,.F.,.F.,.F.,(4,1,1,4),(4,4),(0.,0.285714285714286,0.571428571428571,
1.),(-0.00421817271916687,0.124025126494243),.UNSPECIFIED.);
#165=B_SPLINE_SURFACE_WITH_KNOTS('',3,3,((#13819,#13820,#13821,#13822),
(#13823,#13824,#13825,#13826),(#13827,#13828,#13829,#13830),(#13831,#13832,
#13833,#13834),(#13835,#13836,#13837,#13838)),.UNSPECIFIED.,.F.,.F.,.F.,
(4,1,4),(4,4),(0.,0.571428571428571,1.),(-0.00306862226109154,0.124708996851356),
 .UNSPECIFIED.);
#166=B_SPLINE_SURFACE_WITH_KNOTS('',3,3,((#13872,#13873,#13874,#13875),
(#13876,#13877,#13878,#13879),(#13880,#13881,#13882,#13883),(#13884,#13885,
#13886,#13887),(#13888,#13889,#13890,#13891),(#13892,#13893,#13894,#13895)),
 .UNSPECIFIED.,.F.,.F.,.F.,(4,1,1,4),(4,4),(0.,0.285714285714286,0.571428571428571,
1.),(-0.00430078538920315,0.12402512649425),.UNSPECIFIED.);
#167=B_SPLINE_SURFACE_WITH_KNOTS('',3,3,((#13940,#13941,#13942,#13943),
(#13944,#13945,#13946,#13947),(#13948,#13949,#13950,#13951),(#13952,#13953,
#13954,#13955)),.UNSPECIFIED.,.F.,.F.,.F.,(4,4),(4,4),(0.0133790898038168,
0.988310034964378),(0.,0.621418053491537),.UNSPECIFIED.);
#168=B_SPLINE_SURFACE_WITH_KNOTS('',3,3,((#16338,#16339,#16340,#16341,#16342,
#16343,#16344,#16345,#16346,#16347,#16348,#16349,#16350,#16351,#16352,#16353,
#16354,#16355,#16356,#16357,#16358,#16359,#16360,#16361,#16362,#16363,#16364,
#16365,#16366,#16367,#16368,#16369,#16370,#16371,#16372,#16373,#16374,#16375,
#16376,#16377,#16378,#16379,#16380,#16381,#16382,#16383,#16384,#16385,#16386,
#16387,#16388,#16389,#16390,#16391,#16392,#16393,#16394,#16395,#16396,#16397,
#16398,#16399,#16400,#16401,#16402,#16403,#16404,#16405,#16406,#16407,#16408,
#16409,#16410,#16411,#16412,#16413,#16414,#16415,#16416,#16417,#16418,#16419,
#16420,#16421,#16422,#16423,#16424,#16425,#16426,#16427,#16428,#16429,#16430,
#16431,#16432,#16433,#16434,#16435,#16436,#16437,#16438,#16439,#16440,#16441,
#16442,#16443,#16444,#16445,#16446,#16447,#16448,#16449,#16450,#16451,#16452,
#16453,#16454,#16455,#16456,#16457,#16458,#16459,#16460,#16461,#16462,#16463,
#16464,#16465,#16466,#16467,#16468,#16469,#16470,#16471,#16472,#16473,#16474,
#16475,#16476,#16477,#16478,#16479,#16480,#16481,#16482,#16483,#16484,#16485,
#16486,#16487,#16488,#16489,#16490,#16491,#16492,#16493,#16494,#16495,#16496,
#16497,#16498,#16499,#16500,#16501,#16502,#16503,#16504,#16505,#16506,#16507,
#16508,#16509,#16510,#16511,#16512,#16513,#16514,#16515,#16516,#16517,#16518,
#16519,#16520,#16521,#16522,#16523,#16524,#16525,#16526,#16527,#16528,#16529,
#16530,#16531,#16532,#16533),(#16534,#16535,#16536,#16537,#16538,#16539,
#16540,#16541,#16542,#16543,#16544,#16545,#16546,#16547,#16548,#16549,#16550,
#16551,#16552,#16553,#16554,#16555,#16556,#16557,#16558,#16559,#16560,#16561,
#16562,#16563,#16564,#16565,#16566,#16567,#16568,#16569,#16570,#16571,#16572,
#16573,#16574,#16575,#16576,#16577,#16578,#16579,#16580,#16581,#16582,#16583,
#16584,#16585,#16586,#16587,#16588,#16589,#16590,#16591,#16592,#16593,#16594,
#16595,#16596,#16597,#16598,#16599,#16600,#16601,#16602,#16603,#16604,#16605,
#16606,#16607,#16608,#16609,#16610,#16611,#16612,#16613,#16614,#16615,#16616,
#16617,#16618,#16619,#16620,#16621,#16622,#16623,#16624,#16625,#16626,#16627,
#16628,#16629,#16630,#16631,#16632,#16633,#16634,#16635,#16636,#16637,#16638,
#16639,#16640,#16641,#16642,#16643,#16644,#16645,#16646,#16647,#16648,#16649,
#16650,#16651,#16652,#16653,#16654,#16655,#16656,#16657,#16658,#16659,#16660,
#16661,#16662,#16663,#16664,#16665,#16666,#16667,#16668,#16669,#16670,#16671,
#16672,#16673,#16674,#16675,#16676,#16677,#16678,#16679,#16680,#16681,#16682,
#16683,#16684,#16685,#16686,#16687,#16688,#16689,#16690,#16691,#16692,#16693,
#16694,#16695,#16696,#16697,#16698,#16699,#16700,#16701,#16702,#16703,#16704,
#16705,#16706,#16707,#16708,#16709,#16710,#16711,#16712,#16713,#16714,#16715,
#16716,#16717,#16718,#16719,#16720,#16721,#16722,#16723,#16724,#16725,#16726,
#16727,#16728,#16729),(#16730,#16731,#16732,#16733,#16734,#16735,#16736,
#16737,#16738,#16739,#16740,#16741,#16742,#16743,#16744,#16745,#16746,#16747,
#16748,#16749,#16750,#16751,#16752,#16753,#16754,#16755,#16756,#16757,#16758,
#16759,#16760,#16761,#16762,#16763,#16764,#16765,#16766,#16767,#16768,#16769,
#16770,#16771,#16772,#16773,#16774,#16775,#16776,#16777,#16778,#16779,#16780,
#16781,#16782,#16783,#16784,#16785,#16786,#16787,#16788,#16789,#16790,#16791,
#16792,#16793,#16794,#16795,#16796,#16797,#16798,#16799,#16800,#16801,#16802,
#16803,#16804,#16805,#16806,#16807,#16808,#16809,#16810,#16811,#16812,#16813,
#16814,#16815,#16816,#16817,#16818,#16819,#16820,#16821,#16822,#16823,#16824,
#16825,#16826,#16827,#16828,#16829,#16830,#16831,#16832,#16833,#16834,#16835,
#16836,#16837,#16838,#16839,#16840,#16841,#16842,#16843,#16844,#16845,#16846,
#16847,#16848,#16849,#16850,#16851,#16852,#16853,#16854,#16855,#16856,#16857,
#16858,#16859,#16860,#16861,#16862,#16863,#16864,#16865,#16866,#16867,#16868,
#16869,#16870,#16871,#16872,#16873,#16874,#16875,#16876,#16877,#16878,#16879,
#16880,#16881,#16882,#16883,#16884,#16885,#16886,#16887,#16888,#16889,#16890,
#16891,#16892,#16893,#16894,#16895,#16896,#16897,#16898,#16899,#16900,#16901,
#16902,#16903,#16904,#16905,#16906,#16907,#16908,#16909,#16910,#16911,#16912,
#16913,#16914,#16915,#16916,#16917,#16918,#16919,#16920,#16921,#16922,#16923,
#16924,#16925),(#16926,#16927,#16928,#16929,#16930,#16931,#16932,#16933,
#16934,#16935,#16936,#16937,#16938,#16939,#16940,#16941,#16942,#16943,#16944,
#16945,#16946,#16947,#16948,#16949,#16950,#16951,#16952,#16953,#16954,#16955,
#16956,#16957,#16958,#16959,#16960,#16961,#16962,#16963,#16964,#16965,#16966,
#16967,#16968,#16969,#16970,#16971,#16972,#16973,#16974,#16975,#16976,#16977,
#16978,#16979,#16980,#16981,#16982,#16983,#16984,#16985,#16986,#16987,#16988,
#16989,#16990,#16991,#16992,#16993,#16994,#16995,#16996,#16997,#16998,#16999,
#17000,#17001,#17002,#17003,#17004,#17005,#17006,#17007,#17008,#17009,#17010,
#17011,#17012,#17013,#17014,#17015,#17016,#17017,#17018,#17019,#17020,#17021,
#17022,#17023,#17024,#17025,#17026,#17027,#17028,#17029,#17030,#17031,#17032,
#17033,#17034,#17035,#17036,#17037,#17038,#17039,#17040,#17041,#17042,#17043,
#17044,#17045,#17046,#17047,#17048,#17049,#17050,#17051,#17052,#17053,#17054,
#17055,#17056,#17057,#17058,#17059,#17060,#17061,#17062,#17063,#17064,#17065,
#17066,#17067,#17068,#17069,#17070,#17071,#17072,#17073,#17074,#17075,#17076,
#17077,#17078,#17079,#17080,#17081,#17082,#17083,#17084,#17085,#17086,#17087,
#17088,#17089,#17090,#17091,#17092,#17093,#17094,#17095,#17096,#17097,#17098,
#17099,#17100,#17101,#17102,#17103,#17104,#17105,#17106,#17107,#17108,#17109,
#17110,#17111,#17112,#17113,#17114,#17115,#17116,#17117,#17118,#17119,#17120,
#17121)),.UNSPECIFIED.,.F.,.F.,.F.,(4,4),(4,1,1,1,1,1,1,1,1,1,1,1,1,1,1,
1,1,1,1,1,1,1,1,1,1,1,1,1,1,1,1,1,1,1,1,1,1,1,1,1,1,1,1,1,1,1,1,1,1,1,1,
1,1,1,1,1,1,1,1,1,1,1,1,1,1,1,1,1,1,1,1,1,1,1,1,1,1,1,1,1,1,1,1,1,1,1,1,
1,1,1,1,1,1,1,1,1,1,1,1,1,1,1,1,1,1,1,1,1,1,1,1,1,1,1,1,1,1,1,1,1,1,1,1,
1,1,1,1,1,1,1,1,1,1,1,1,1,1,1,1,1,1,1,1,1,1,1,1,1,1,1,1,1,1,1,1,1,1,1,1,
1,1,1,1,1,1,1,1,1,1,1,1,1,1,1,1,1,1,1,1,1,1,1,1,1,1,1,1,1,1,1,1,1,1,4),
(0.,0.0329955678841871),(11.6159397475006,12.61358260836,13.6112254692194,
14.6088683300789,15.6065111909383,16.6041540517977,17.6017969126571,18.5994397735165,
19.5970826343759,20.5947254952353,21.5923683560947,22.5900112169541,23.5876540778135,
24.5852969386729,25.5829397995323,26.5805826603917,27.5782255212511,28.5758683821105,
29.5735112429699,30.5711541038294,31.5687969646888,32.5664398255482,33.5640826864076,
34.561725547267,35.5593684081264,36.5570112689858,37.5546541298452,38.5522969907046,
39.549939851564,40.5475827124234,41.5452255732828,42.5428684341422,43.5405112950016,
44.538154155861,45.5357970167204,46.5334398775799,47.5310827384393,48.5287255992987,
49.5263684601581,50.5240113210175,51.5216541818769,52.5192970427363,53.5169399035957,
54.5145827644551,55.5122256253145,56.5098684861739,57.5075113470333,58.5051542078927,
59.5027970687521,60.5004399296115,61.4980827904709,62.4957256513303,63.4933685121897,
64.4910113730492,65.4886542339086,66.486297094768,67.4839399556274,68.4815828164868,
69.4792256773462,70.4768685382056,71.474511399065,72.4721542599244,73.4697971207838,
74.4674399816432,75.4650828425026,76.462725703362,77.4603685642214,78.4580114250808,
79.4556542859402,80.4532971467996,81.4509400076591,82.4485828685185,83.4462257293779,
84.4438685902373,85.4415114510967,86.4391543119561,87.4367971728155,88.4344400336749,
89.4320828945343,90.4297257553937,91.4273686162531,92.4250114771125,93.4226543379719,
94.4202971988313,95.4179400596907,96.4155829205502,97.4132257814096,98.410868642269,
99.4085115031284,100.406154363988,101.403797224847,102.401440085707,103.399082946566,
104.396725807425,105.394368668285,106.392011529144,107.389654390004,108.387297250863,
109.384940111722,110.382582972582,111.380225833441,112.377868694301,113.37551155516,
114.373154416019,115.370797276879,116.368440137738,117.366082998598,118.363725859457,
119.361368720316,120.359011581176,121.356654442035,122.354297302895,123.351940163754,
124.349583024614,125.347225885473,126.344868746332,127.342511607192,128.340154468051,
129.337797328911,130.33544018977,131.333083050629,132.330725911489,133.328368772348,
134.326011633208,135.323654494067,136.321297354926,137.318940215786,138.316583076645,
139.314225937505,140.311868798364,141.309511659223,142.307154520083,143.304797380942,
144.302440241802,145.300083102661,146.29772596352,147.29536882438,148.293011685239,
149.290654546099,150.288297406958,151.285940267817,152.283583128677,153.281225989536,
154.278868850396,155.276511711255,156.274154572115,157.271797432974,158.269440293833,
159.267083154693,160.264726015552,161.262368876412,162.260011737271,163.25765459813,
164.25529745899,165.252940319849,166.250583180709,167.248226041568,168.245868902427,
169.243511763287,170.241154624146,171.238797485006,172.236440345865,173.234083206724,
174.231726067584,175.229368928443,176.227011789303,177.224654650162,178.222297511021,
179.219940371881,180.21758323274,181.2152260936,182.212868954459,183.210511815318,
184.208154676178,185.205797537037,186.203440397897,187.201083258756,188.198726119616,
189.196368980475,190.194011841334,191.191654702194,192.189297563053,193.186940423913,
194.184583284772,195.182226145631,196.179869006491,197.17751186735,198.17515472821,
199.172797589069,200.170440449928,201.168083310788,202.165726171647,203.163369032507,
204.161011893366),.UNSPECIFIED.);
#169=B_SPLINE_SURFACE_WITH_KNOTS('',3,3,((#17211,#17212,#17213,#17214,#17215,
#17216,#17217,#17218,#17219,#17220,#17221,#17222,#17223,#17224,#17225,#17226,
#17227,#17228,#17229,#17230,#17231,#17232,#17233,#17234,#17235,#17236,#17237,
#17238,#17239,#17240,#17241,#17242,#17243,#17244,#17245,#17246,#17247,#17248,
#17249,#17250,#17251,#17252,#17253,#17254,#17255,#17256,#17257,#17258,#17259,
#17260,#17261,#17262,#17263,#17264,#17265,#17266,#17267,#17268,#17269,#17270,
#17271,#17272,#17273,#17274,#17275,#17276,#17277,#17278,#17279,#17280,#17281,
#17282,#17283,#17284,#17285,#17286,#17287,#17288,#17289,#17290,#17291,#17292,
#17293,#17294,#17295,#17296,#17297,#17298,#17299,#17300,#17301,#17302,#17303,
#17304,#17305,#17306,#17307,#17308,#17309,#17310,#17311,#17312,#17313,#17314,
#17315,#17316,#17317,#17318,#17319,#17320,#17321,#17322,#17323,#17324,#17325,
#17326,#17327,#17328,#17329,#17330,#17331,#17332,#17333,#17334,#17335,#17336,
#17337,#17338,#17339,#17340,#17341,#17342,#17343,#17344,#17345,#17346,#17347,
#17348,#17349,#17350,#17351,#17352,#17353,#17354,#17355,#17356,#17357,#17358,
#17359,#17360,#17361,#17362,#17363,#17364,#17365,#17366,#17367,#17368,#17369,
#17370,#17371,#17372,#17373,#17374,#17375,#17376,#17377,#17378,#17379,#17380,
#17381,#17382,#17383,#17384,#17385,#17386,#17387,#17388,#17389,#17390,#17391,
#17392,#17393,#17394,#17395,#17396,#17397,#17398,#17399,#17400,#17401,#17402,
#17403,#17404,#17405,#17406,#17407,#17408),(#17409,#17410,#17411,#17412,
#17413,#17414,#17415,#17416,#17417,#17418,#17419,#17420,#17421,#17422,#17423,
#17424,#17425,#17426,#17427,#17428,#17429,#17430,#17431,#17432,#17433,#17434,
#17435,#17436,#17437,#17438,#17439,#17440,#17441,#17442,#17443,#17444,#17445,
#17446,#17447,#17448,#17449,#17450,#17451,#17452,#17453,#17454,#17455,#17456,
#17457,#17458,#17459,#17460,#17461,#17462,#17463,#17464,#17465,#17466,#17467,
#17468,#17469,#17470,#17471,#17472,#17473,#17474,#17475,#17476,#17477,#17478,
#17479,#17480,#17481,#17482,#17483,#17484,#17485,#17486,#17487,#17488,#17489,
#17490,#17491,#17492,#17493,#17494,#17495,#17496,#17497,#17498,#17499,#17500,
#17501,#17502,#17503,#17504,#17505,#17506,#17507,#17508,#17509,#17510,#17511,
#17512,#17513,#17514,#17515,#17516,#17517,#17518,#17519,#17520,#17521,#17522,
#17523,#17524,#17525,#17526,#17527,#17528,#17529,#17530,#17531,#17532,#17533,
#17534,#17535,#17536,#17537,#17538,#17539,#17540,#17541,#17542,#17543,#17544,
#17545,#17546,#17547,#17548,#17549,#17550,#17551,#17552,#17553,#17554,#17555,
#17556,#17557,#17558,#17559,#17560,#17561,#17562,#17563,#17564,#17565,#17566,
#17567,#17568,#17569,#17570,#17571,#17572,#17573,#17574,#17575,#17576,#17577,
#17578,#17579,#17580,#17581,#17582,#17583,#17584,#17585,#17586,#17587,#17588,
#17589,#17590,#17591,#17592,#17593,#17594,#17595,#17596,#17597,#17598,#17599,
#17600,#17601,#17602,#17603,#17604,#17605,#17606),(#17607,#17608,#17609,
#17610,#17611,#17612,#17613,#17614,#17615,#17616,#17617,#17618,#17619,#17620,
#17621,#17622,#17623,#17624,#17625,#17626,#17627,#17628,#17629,#17630,#17631,
#17632,#17633,#17634,#17635,#17636,#17637,#17638,#17639,#17640,#17641,#17642,
#17643,#17644,#17645,#17646,#17647,#17648,#17649,#17650,#17651,#17652,#17653,
#17654,#17655,#17656,#17657,#17658,#17659,#17660,#17661,#17662,#17663,#17664,
#17665,#17666,#17667,#17668,#17669,#17670,#17671,#17672,#17673,#17674,#17675,
#17676,#17677,#17678,#17679,#17680,#17681,#17682,#17683,#17684,#17685,#17686,
#17687,#17688,#17689,#17690,#17691,#17692,#17693,#17694,#17695,#17696,#17697,
#17698,#17699,#17700,#17701,#17702,#17703,#17704,#17705,#17706,#17707,#17708,
#17709,#17710,#17711,#17712,#17713,#17714,#17715,#17716,#17717,#17718,#17719,
#17720,#17721,#17722,#17723,#17724,#17725,#17726,#17727,#17728,#17729,#17730,
#17731,#17732,#17733,#17734,#17735,#17736,#17737,#17738,#17739,#17740,#17741,
#17742,#17743,#17744,#17745,#17746,#17747,#17748,#17749,#17750,#17751,#17752,
#17753,#17754,#17755,#17756,#17757,#17758,#17759,#17760,#17761,#17762,#17763,
#17764,#17765,#17766,#17767,#17768,#17769,#17770,#17771,#17772,#17773,#17774,
#17775,#17776,#17777,#17778,#17779,#17780,#17781,#17782,#17783,#17784,#17785,
#17786,#17787,#17788,#17789,#17790,#17791,#17792,#17793,#17794,#17795,#17796,
#17797,#17798,#17799,#17800,#17801,#17802,#17803,#17804),(#17805,#17806,
#17807,#17808,#17809,#17810,#17811,#17812,#17813,#17814,#17815,#17816,#17817,
#17818,#17819,#17820,#17821,#17822,#17823,#17824,#17825,#17826,#17827,#17828,
#17829,#17830,#17831,#17832,#17833,#17834,#17835,#17836,#17837,#17838,#17839,
#17840,#17841,#17842,#17843,#17844,#17845,#17846,#17847,#17848,#17849,#17850,
#17851,#17852,#17853,#17854,#17855,#17856,#17857,#17858,#17859,#17860,#17861,
#17862,#17863,#17864,#17865,#17866,#17867,#17868,#17869,#17870,#17871,#17872,
#17873,#17874,#17875,#17876,#17877,#17878,#17879,#17880,#17881,#17882,#17883,
#17884,#17885,#17886,#17887,#17888,#17889,#17890,#17891,#17892,#17893,#17894,
#17895,#17896,#17897,#17898,#17899,#17900,#17901,#17902,#17903,#17904,#17905,
#17906,#17907,#17908,#17909,#17910,#17911,#17912,#17913,#17914,#17915,#17916,
#17917,#17918,#17919,#17920,#17921,#17922,#17923,#17924,#17925,#17926,#17927,
#17928,#17929,#17930,#17931,#17932,#17933,#17934,#17935,#17936,#17937,#17938,
#17939,#17940,#17941,#17942,#17943,#17944,#17945,#17946,#17947,#17948,#17949,
#17950,#17951,#17952,#17953,#17954,#17955,#17956,#17957,#17958,#17959,#17960,
#17961,#17962,#17963,#17964,#17965,#17966,#17967,#17968,#17969,#17970,#17971,
#17972,#17973,#17974,#17975,#17976,#17977,#17978,#17979,#17980,#17981,#17982,
#17983,#17984,#17985,#17986,#17987,#17988,#17989,#17990,#17991,#17992,#17993,
#17994,#17995,#17996,#17997,#17998,#17999,#18000,#18001,#18002)),
 .UNSPECIFIED.,.F.,.F.,.F.,(4,4),(4,1,1,1,1,1,1,1,1,1,1,1,1,1,1,1,1,1,1,
1,1,1,1,1,1,1,1,1,1,1,1,1,1,1,1,1,1,1,1,1,1,1,1,1,1,1,1,1,1,1,1,1,1,1,1,
1,1,1,1,1,1,1,1,1,1,1,1,1,1,1,1,1,1,1,1,1,1,1,1,1,1,1,1,1,1,1,1,1,1,1,1,
1,1,1,1,1,1,1,1,1,1,1,1,1,1,1,1,1,1,1,1,1,1,1,1,1,1,1,1,1,1,1,1,1,1,1,1,
1,1,1,1,1,1,1,1,1,1,1,1,1,1,1,1,1,1,1,1,1,1,1,1,1,1,1,1,1,1,1,1,1,1,1,1,
1,1,1,1,1,1,1,1,1,1,1,1,1,1,1,1,1,1,1,1,1,1,1,1,1,1,1,1,1,1,1,1,4),(0.,
0.0329955678841871),(8.30203615430855,9.30007843543257,10.2981207165566,
11.2961629976806,12.2942052788047,13.2922475599287,14.2902898410527,15.2883321221767,
16.2863744033008,17.2844166844248,18.2824589655488,19.2805012466728,20.2785435277969,
21.2765858089209,22.2746280900449,23.272670371169,24.270712652293,25.268754933417,
26.266797214541,27.2648394956651,28.2628817767891,29.2609240579131,30.2589663390371,
31.2570086201612,32.2550509012852,33.2530931824092,34.2511354635333,35.2491777446573,
36.2472200257813,37.2452623069053,38.2433045880294,39.2413468691534,40.2393891502774,
41.2374314314014,42.2354737125255,43.2335159936495,44.2315582747735,45.2296005558975,
46.2276428370216,47.2256851181456,48.2237273992696,49.2217696803937,50.2198119615177,
51.2178542426417,52.2158965237657,53.2139388048898,54.2119810860138,55.2100233671378,
56.2080656482619,57.2061079293859,58.2041502105099,59.2021924916339,60.200234772758,
61.198277053882,62.196319335006,63.19436161613,64.1924038972541,65.1904461783781,
66.1884884595021,67.1865307406262,68.1845730217502,69.1826153028742,70.1806575839982,
71.1786998651223,72.1767421462463,73.1747844273703,74.1728267084943,75.1708689896184,
76.1689112707424,77.1669535518664,78.1649958329905,79.1630381141145,80.1610803952385,
81.1591226763625,82.1571649574865,83.1552072386106,84.1532495197346,85.1512918008586,
86.1493340819827,87.1473763631067,88.1454186442307,89.1434609253548,90.1415032064788,
91.1395454876028,92.1375877687268,93.1356300498508,94.1336723309749,95.1317146120989,
96.1297568932229,97.127799174347,98.125841455471,99.123883736595,100.121926017719,
101.119968298843,102.118010579967,103.116052861091,104.114095142215,105.112137423339,
106.110179704463,107.108221985587,108.106264266711,109.104306547835,110.102348828959,
111.100391110083,112.098433391207,113.096475672331,114.094517953455,115.092560234579,
116.090602515703,117.088644796828,118.086687077952,119.084729359076,120.0827716402,
121.080813921324,122.078856202448,123.076898483572,124.074940764696,125.07298304582,
126.071025326944,127.069067608068,128.067109889192,129.065152170316,130.06319445144,
131.061236732564,132.059279013688,133.057321294812,134.055363575936,135.05340585706,
136.051448138184,137.049490419308,138.047532700432,139.045574981556,140.04361726268,
141.041659543804,142.039701824928,143.037744106052,144.035786387176,145.0338286683,
146.031870949424,147.029913230548,148.027955511672,149.025997792796,150.02404007392,
151.022082355044,152.020124636168,153.018166917292,154.016209198417,155.014251479541,
156.012293760665,157.010336041789,158.008378322913,159.006420604037,160.004462885161,
161.002505166285,162.000547447409,162.998589728533,163.996632009657,164.994674290781,
165.992716571905,166.990758853029,167.988801134153,168.986843415277,169.984885696401,
170.982927977525,171.980970258649,172.979012539773,173.977054820897,174.975097102021,
175.973139383145,176.971181664269,177.969223945393,178.967266226517,179.965308507641,
180.963350788765,181.961393069889,182.959435351013,183.957477632137,184.955519913261,
185.953562194385,186.951604475509,187.949646756633,188.947689037757,189.945731318881,
190.943773600006,191.94181588113,192.939858162254,193.937900443378,194.935942724502,
195.933985005626,196.93202728675,197.930069567874,198.928111848998,199.926154130122,
200.924196411246,201.92223869237,202.920280973494),.UNSPECIFIED.);
#170=B_SPLINE_SURFACE_WITH_KNOTS('',3,3,((#18461,#18462,#18463,#18464,#18465,
#18466,#18467,#18468,#18469,#18470,#18471,#18472,#18473,#18474,#18475,#18476,
#18477,#18478,#18479,#18480,#18481,#18482,#18483,#18484,#18485,#18486,#18487,
#18488,#18489,#18490,#18491,#18492,#18493,#18494,#18495,#18496),(#18497,
#18498,#18499,#18500,#18501,#18502,#18503,#18504,#18505,#18506,#18507,#18508,
#18509,#18510,#18511,#18512,#18513,#18514,#18515,#18516,#18517,#18518,#18519,
#18520,#18521,#18522,#18523,#18524,#18525,#18526,#18527,#18528,#18529,#18530,
#18531,#18532),(#18533,#18534,#18535,#18536,#18537,#18538,#18539,#18540,
#18541,#18542,#18543,#18544,#18545,#18546,#18547,#18548,#18549,#18550,#18551,
#18552,#18553,#18554,#18555,#18556,#18557,#18558,#18559,#18560,#18561,#18562,
#18563,#18564,#18565,#18566,#18567,#18568),(#18569,#18570,#18571,#18572,
#18573,#18574,#18575,#18576,#18577,#18578,#18579,#18580,#18581,#18582,#18583,
#18584,#18585,#18586,#18587,#18588,#18589,#18590,#18591,#18592,#18593,#18594,
#18595,#18596,#18597,#18598,#18599,#18600,#18601,#18602,#18603,#18604)),
 .UNSPECIFIED.,.F.,.F.,.F.,(4,4),(4,1,1,1,1,1,1,1,1,1,1,1,1,1,1,1,1,1,1,
1,1,1,1,1,1,1,1,1,1,1,1,1,1,4),(0.,0.0321584099938622),(11.8553612635794,
12.830508595889,13.8056559281987,14.7808032605084,15.755950592818,16.7310979251277,
17.7062452574374,18.681392589747,19.6565399220567,20.6316872543664,21.606834586676,
22.5819819189857,23.5571292512954,24.532276583605,25.5074239159147,26.4825712482243,
27.457718580534,28.4328659128437,29.4080132451533,30.383160577463,31.3583079097727,
32.3334552420823,33.308602574392,34.2837499067017,35.2588972390113,36.234044571321,
37.2091919036307,38.1843392359403,39.15948656825,40.1346339005596,41.1097812328693,
42.084928565179,43.0600758974886,44.0352232297983),.UNSPECIFIED.);
#171=B_SPLINE_SURFACE_WITH_KNOTS('',3,3,((#18728,#18729,#18730,#18731,#18732,
#18733,#18734,#18735,#18736,#18737,#18738,#18739,#18740,#18741,#18742,#18743,
#18744,#18745,#18746,#18747,#18748,#18749,#18750,#18751,#18752,#18753,#18754,
#18755,#18756,#18757,#18758,#18759,#18760,#18761,#18762,#18763),(#18764,
#18765,#18766,#18767,#18768,#18769,#18770,#18771,#18772,#18773,#18774,#18775,
#18776,#18777,#18778,#18779,#18780,#18781,#18782,#18783,#18784,#18785,#18786,
#18787,#18788,#18789,#18790,#18791,#18792,#18793,#18794,#18795,#18796,#18797,
#18798,#18799),(#18800,#18801,#18802,#18803,#18804,#18805,#18806,#18807,
#18808,#18809,#18810,#18811,#18812,#18813,#18814,#18815,#18816,#18817,#18818,
#18819,#18820,#18821,#18822,#18823,#18824,#18825,#18826,#18827,#18828,#18829,
#18830,#18831,#18832,#18833,#18834,#18835),(#18836,#18837,#18838,#18839,
#18840,#18841,#18842,#18843,#18844,#18845,#18846,#18847,#18848,#18849,#18850,
#18851,#18852,#18853,#18854,#18855,#18856,#18857,#18858,#18859,#18860,#18861,
#18862,#18863,#18864,#18865,#18866,#18867,#18868,#18869,#18870,#18871)),
 .UNSPECIFIED.,.F.,.F.,.F.,(4,4),(4,1,1,1,1,1,1,1,1,1,1,1,1,1,1,1,1,1,1,
1,1,1,1,1,1,1,1,1,1,1,1,1,1,4),(0.,0.0321584099938622),(14.3984001269719,
15.3735474592815,16.3486947915912,17.3238421239009,18.2989894562105,19.2741367885202,
20.2492841208299,21.2244314531395,22.1995787854492,23.1747261177589,24.1498734500685,
25.1250207823782,26.1001681146879,27.0753154469975,28.0504627793072,29.0256101116168,
30.0007574439265,30.9759047762362,31.9510521085458,32.9261994408555,33.9013467731652,
34.8764941054748,35.8516414377845,36.8267887700942,37.8019361024038,38.7770834347135,
39.7522307670232,40.7273780993328,41.7025254316425,42.6776727639522,43.6528200962618,
44.6279674285715,45.6031147608811,46.5782620931908),.UNSPECIFIED.);
#172=B_SPLINE_CURVE_WITH_KNOTS('',3,(#9197,#9198,#9199,#9200),
 .UNSPECIFIED.,.F.,.F.,(4,4),(3.28016616408593,4.26236080300681),
 .UNSPECIFIED.);
#173=B_SPLINE_CURVE_WITH_KNOTS('',3,(#9204,#9205,#9206,#9207),
 .UNSPECIFIED.,.F.,.F.,(4,4),(8.92392608805945,9.90612072688831),
 .UNSPECIFIED.);
#174=B_SPLINE_CURVE_WITH_KNOTS('',3,(#9209,#9210,#9211,#9212,#9213,#9214,
#9215,#9216,#9217,#9218,#9219,#9220,#9221,#9222,#9223,#9224,#9225,#9226,
#9227),.UNSPECIFIED.,.F.,.F.,(4,3,3,3,3,3,4),(-0.050768112872884,-0.0388528786649772,
-0.0311058171716578,-0.0259830388669653,-0.0210744122964195,-0.0143837148934404,
0.),.UNSPECIFIED.);
#175=B_SPLINE_CURVE_WITH_KNOTS('',3,(#9229,#9230,#9231,#9232),
 .UNSPECIFIED.,.F.,.F.,(4,4),(9.9568018127159,12.1251256661408),
 .UNSPECIFIED.);
#176=B_SPLINE_CURVE_WITH_KNOTS('',3,(#9236,#9237,#9238,#9239),
 .UNSPECIFIED.,.F.,.F.,(4,4),(1.06116122492545,3.22948508825557),
 .UNSPECIFIED.);
#177=B_SPLINE_CURVE_WITH_KNOTS('',3,(#9240,#9241,#9242,#9243,#9244,#9245,
#9246,#9247,#9248,#9249,#9250,#9251,#9252,#9253,#9254,#9255,#9256,#9257,
#9258),.UNSPECIFIED.,.F.,.F.,(4,3,3,3,3,3,4),(-0.0507681129736439,-0.0388528772897764,
-0.0311058147321604,-0.0259830361493327,-0.0210744097201194,-0.0143837130754026,
-9.90506278315E-9),.UNSPECIFIED.);
#178=B_SPLINE_CURVE_WITH_KNOTS('',3,(#9406,#9407,#9408,#9409,#9410,#9411),
 .UNSPECIFIED.,.F.,.F.,(4,2,4),(-0.605566356596631,-0.303329629920269,-0.000148729590407126),
 .UNSPECIFIED.);
#179=B_SPLINE_CURVE_WITH_KNOTS('',3,(#9413,#9414,#9415,#9416,#9417,#9418,
#9419,#9420,#9421,#9422,#9423,#9424,#9425,#9426,#9427,#9428,#9429,#9430,
#9431,#9432,#9433,#9434,#9435,#9436,#9437,#9438,#9439,#9440),
 .UNSPECIFIED.,.F.,.F.,(4,3,3,3,3,3,3,3,3,4),(-0.153210533292091,-0.129383071834804,
-0.117098895005168,-0.0931297672424715,-0.0778761857300216,-0.065564095006876,
-0.0417435583396367,-0.038874550231651,-0.0150983388519663,0.),
 .UNSPECIFIED.);
#180=B_SPLINE_CURVE_WITH_KNOTS('',3,(#9444,#9445,#9446,#9447,#9448,#9449,
#9450,#9451,#9452,#9453,#9454,#9455,#9456,#9457,#9458,#9459,#9460,#9461,
#9462,#9463,#9464,#9465,#9466,#9467,#9468,#9469,#9470,#9471),
 .UNSPECIFIED.,.F.,.F.,(4,3,3,3,3,3,3,3,3,4),(-0.153244081227051,-0.129493605146206,
-0.117970006482883,-0.0941492904140308,-0.0876825809854227,-0.078828741443105,
-0.0548877675055393,-0.0394694906046094,-0.0155984926894347,0.),
 .UNSPECIFIED.);
#181=B_SPLINE_CURVE_WITH_KNOTS('',3,(#9472,#9473,#9474,#9475,#9476,#9477),
 .UNSPECIFIED.,.F.,.F.,(4,2,4),(-0.606539490527658,-0.303329031627741,-0.00112184825655631),
 .UNSPECIFIED.);
#182=B_SPLINE_CURVE_WITH_KNOTS('',3,(#9482,#9483,#9484,#9485,#9486,#9487),
 .UNSPECIFIED.,.F.,.F.,(4,2,4),(-0.606785247764818,-0.303663188081886,-0.00088649083675002),
 .UNSPECIFIED.);
#183=B_SPLINE_CURVE_WITH_KNOTS('',3,(#9489,#9490,#9491,#9492,#9493,#9494,
#9495,#9496,#9497,#9498,#9499,#9500,#9501,#9502,#9503,#9504,#9505,#9506,
#9507,#9508,#9509,#9510,#9511,#9512,#9513,#9514,#9515,#9516),
 .UNSPECIFIED.,.F.,.F.,(4,3,3,3,3,3,3,3,3,4),(-0.15258577077829,-0.128839317352572,
-0.117158786685373,-0.0932148261566644,-0.0780319390000633,-0.0653676349965338,
-0.0415665498371782,-0.0389909618069961,-0.0152059030050533,0.),
 .UNSPECIFIED.);
#184=B_SPLINE_CURVE_WITH_KNOTS('',3,(#9520,#9521,#9522,#9523,#9524,#9525,
#9526,#9527,#9528,#9529,#9530,#9531,#9532,#9533,#9534,#9535,#9536,#9537,
#9538,#9539,#9540,#9541,#9542,#9543,#9544,#9545,#9546,#9547),
 .UNSPECIFIED.,.F.,.F.,(4,3,3,3,3,3,3,3,3,4),(-0.152596853546747,-0.128825864440686,
-0.115507515430042,-0.0917263797372463,-0.0872428123353572,-0.0783995504057471,
-0.0544835945915644,-0.0392209901554083,-0.0154275313391792,0.),
 .UNSPECIFIED.);
#185=B_SPLINE_CURVE_WITH_KNOTS('',3,(#9549,#9550,#9551,#9552,#9553,#9554),
 .UNSPECIFIED.,.F.,.F.,(4,2,4),(-0.606440835737524,-0.303663090452391,-0.000542069086802599),
 .UNSPECIFIED.);
#186=B_SPLINE_CURVE_WITH_KNOTS('',3,(#9560,#9561,#9562,#9563,#9564,#9565),
 .UNSPECIFIED.,.F.,.F.,(4,2,4),(-0.607379220946441,-0.303761646676304,-0.00124422999587004),
 .UNSPECIFIED.);
#187=B_SPLINE_CURVE_WITH_KNOTS('',3,(#9567,#9568,#9569,#9570,#9571,#9572,
#9573,#9574,#9575,#9576,#9577,#9578,#9579,#9580,#9581,#9582,#9583,#9584,
#9585,#9586,#9587,#9588,#9589,#9590,#9591,#9592,#9593,#9594),
 .UNSPECIFIED.,.F.,.F.,(4,3,3,3,3,3,3,3,3,4),(-0.152287640102895,-0.128554450486317,
-0.115193035178751,-0.0912770810520543,-0.0781028969167454,-0.0652733399726575,
-0.0414820896655672,-0.0390446621366508,-0.0152552334863041,0.),
 .UNSPECIFIED.);
#188=B_SPLINE_CURVE_WITH_KNOTS('',3,(#9598,#9599,#9600,#9601,#9602,#9603,
#9604,#9605,#9606,#9607,#9608,#9609,#9610,#9611,#9612,#9613,#9614,#9615,
#9616,#9617,#9618,#9619,#9620,#9621,#9622,#9623,#9624,#9625),
 .UNSPECIFIED.,.F.,.F.,(4,3,3,3,3,3,3,3,3,4),(-0.152291020205185,-0.128517753946702,
-0.115248901231919,-0.0914807886786037,-0.0870359119466785,-0.0782017654295232,
-0.054298407767766,-0.03910658747416,-0.0153486482327859,0.),
 .UNSPECIFIED.);
#189=B_SPLINE_CURVE_WITH_KNOTS('',3,(#9627,#9628,#9629,#9630,#9631,#9632),
 .UNSPECIFIED.,.F.,.F.,(4,2,4),(-0.606279550122448,-0.303761677523001,-0.000144559171857295),
 .UNSPECIFIED.);
#190=B_SPLINE_CURVE_WITH_KNOTS('',3,(#9638,#9639,#9640,#9641,#9642,#9643),
 .UNSPECIFIED.,.F.,.F.,(4,2,4),(-0.607536685592867,-0.303784463250135,-0.00133982193348342),
 .UNSPECIFIED.);
#191=B_SPLINE_CURVE_WITH_KNOTS('',3,(#9644,#9645,#9646,#9647,#9648,#9649,
#9650,#9651,#9652,#9653,#9654,#9655,#9656,#9657,#9658,#9659,#9660,#9661,
#9662,#9663,#9664,#9665,#9666,#9667,#9668,#9669,#9670,#9671),
 .UNSPECIFIED.,.F.,.F.,(4,3,3,3,3,3,3,3,3,4),(-0.152217684890348,-0.128490376540845,
-0.11516578527262,-0.091253137134092,-0.0781160865160423,-0.0652495101170982,
-0.0414606291875136,-0.0390546905501479,-0.015263466236765,0.),
 .UNSPECIFIED.);
#192=B_SPLINE_CURVE_WITH_KNOTS('',3,(#9673,#9674,#9675,#9676,#9677,#9678,
#9679,#9680,#9681,#9682,#9683,#9684,#9685,#9686,#9687,#9688,#9689,#9690,
#9691,#9692,#9693,#9694,#9695,#9696,#9697,#9698,#9699,#9700),
 .UNSPECIFIED.,.F.,.F.,(4,3,3,3,3,3,3,3,3,4),(-0.152219351639196,-0.128444680332832,
-0.115193337419806,-0.0914284185691762,-0.0869890032859244,-0.0781648487722283,
-0.0542647883944502,-0.0390852411900305,-0.0153331469286526,0.),
 .UNSPECIFIED.);
#193=B_SPLINE_CURVE_WITH_KNOTS('',3,(#9702,#9703,#9704,#9705,#9706,#9707),
 .UNSPECIFIED.,.F.,.F.,(4,2,4),(-0.606231877025315,-0.303784501204342,-3.50089943914611E-5),
 .UNSPECIFIED.);
#194=B_SPLINE_CURVE_WITH_KNOTS('',3,(#9713,#9714,#9715,#9716),
 .UNSPECIFIED.,.F.,.F.,(4,4),(0.0108333608245492,0.617725317592517),
 .UNSPECIFIED.);
#195=B_SPLINE_CURVE_WITH_KNOTS('',3,(#9720,#9721,#9722,#9723),
 .UNSPECIFIED.,.F.,.F.,(4,4),(-0.617725317592517,-0.0108333608245492),
 .UNSPECIFIED.);
#196=B_SPLINE_CURVE_WITH_KNOTS('',3,(#9726,#9727,#9728,#9729),
 .UNSPECIFIED.,.F.,.F.,(4,4),(8.65483889175297,12.1899094612697),
 .UNSPECIFIED.);
#197=B_SPLINE_CURVE_WITH_KNOTS('',3,(#9730,#9731,#9732,#9733),
 .UNSPECIFIED.,.F.,.F.,(4,4),(0.491886782059505,4.00844302274363),
 .UNSPECIFIED.);
#198=B_SPLINE_CURVE_WITH_KNOTS('',3,(#9736,#9737,#9738,#9739,#9740,#9741,
#9742,#9743,#9744,#9745),.UNSPECIFIED.,.F.,.F.,(4,3,3,4),(4.20909064274042,
6.3236533433415,8.26419514194387,8.41669725637478),.UNSPECIFIED.);
#199=B_SPLINE_CURVE_WITH_KNOTS('',3,(#9748,#9749,#9750,#9751),
 .UNSPECIFIED.,.F.,.F.,(4,4),(8.61714174069208,11.8187712274298),
 .UNSPECIFIED.);
#200=B_SPLINE_CURVE_WITH_KNOTS('',3,(#9755,#9756,#9757,#9758),
 .UNSPECIFIED.,.F.,.F.,(4,4),(12.0182076143484,12.6179302061492),
 .UNSPECIFIED.);
#201=B_SPLINE_CURVE_WITH_KNOTS('',3,(#9759,#9760,#9761,#9762,#9763,#9764,
#9765,#9766,#9767,#9768,#9769,#9770,#9771,#9772,#9773,#9774,#9775,#9776,
#9777,#9778,#9779,#9780,#9781,#9782,#9783,#9784,#9785,#9786),
 .UNSPECIFIED.,.F.,.F.,(4,3,3,3,3,3,3,3,3,4),(0.,0.023812730958415,0.0390943730497349,
0.0628727645281949,0.0664866407211859,0.0780895647789142,0.102003044086093,
0.117056568347941,0.14081843048439,0.155095961761698),.UNSPECIFIED.);
#202=B_SPLINE_CURVE_WITH_KNOTS('',3,(#9790,#9791,#9792,#9793,#9794,#9795,
#9796,#9797,#9798,#9799,#9800,#9801,#9802,#9803,#9804,#9805,#9806,#9807,
#9808,#9809,#9810,#9811,#9812,#9813,#9814,#9815,#9816,#9817,#9818,#9819,
#9820,#9821,#9822,#9823,#9824,#9825,#9826),.UNSPECIFIED.,.F.,.F.,(4,3,3,
3,3,3,3,3,3,3,3,3,4),(0.,0.0535193130531386,0.107740084455895,0.117281563739951,
0.171478196787188,0.199460035548543,0.234266327019636,0.287962832542679,
0.34249270416273,0.351167719367162,0.408228095477446,0.46132246935065,0.46528847158773),
 .UNSPECIFIED.);
#203=B_SPLINE_CURVE_WITH_KNOTS('',3,(#9828,#9829,#9830,#9831),
 .UNSPECIFIED.,.F.,.F.,(4,4),(0.0221781183199723,0.974834454777906),
 .UNSPECIFIED.);
#204=B_SPLINE_CURVE_WITH_KNOTS('',3,(#9833,#9834,#9835,#9836,#9837,#9838,
#9839,#9840,#9841,#9842,#9843,#9844,#9845,#9846,#9847,#9848,#9849,#9850,
#9851,#9852,#9853,#9854,#9855,#9856,#9857,#9858,#9859,#9860,#9861,#9862,
#9863,#9864,#9865,#9866,#9867,#9868,#9869,#9870,#9871,#9872,#9873,#9874,
#9875),.UNSPECIFIED.,.F.,.F.,(4,3,3,3,3,3,3,3,3,3,3,3,3,3,4),(0.,0.0533317239385299,
0.107762434368039,0.117305236535198,0.171635266834242,0.216430402805854,
0.234303130921432,0.288010415584935,0.341932185058889,0.351200358601802,
0.360578786332496,0.414653942238971,0.427906071157934,0.482008506259547,
0.504658879840573),.UNSPECIFIED.);
#205=B_SPLINE_CURVE_WITH_KNOTS('',3,(#9879,#9880,#9881,#9882,#9883,#9884,
#9885,#9886,#9887,#9888,#9889,#9890,#9891,#9892,#9893,#9894,#9895,#9896,
#9897,#9898,#9899,#9900,#9901,#9902,#9903,#9904,#9905,#9906,#9907,#9908,
#9909,#9910,#9911,#9912,#9913,#9914,#9915,#9916,#9917,#9918,#9919,#9920,
#9921),.UNSPECIFIED.,.F.,.F.,(4,3,3,3,3,3,3,3,3,3,3,3,3,3,4),(0.,0.0533492049661439,
0.107791770949794,0.117401360885473,0.171729175646356,0.216477851539682,
0.234467324023732,0.288191829779795,0.342104640447882,0.351366010290958,
0.360619117109406,0.414688080797906,0.427993719046535,0.482081475021072,
0.504664253934307),.UNSPECIFIED.);
#206=B_SPLINE_CURVE_WITH_KNOTS('',3,(#9923,#9924,#9925,#9926),
 .UNSPECIFIED.,.F.,.F.,(4,4),(0.0251655452220943,0.977821881680028),
 .UNSPECIFIED.);
#207=B_SPLINE_CURVE_WITH_KNOTS('',3,(#9928,#9929,#9930,#9931,#9932,#9933,
#9934,#9935,#9936,#9937,#9938,#9939,#9940,#9941,#9942,#9943,#9944,#9945,
#9946,#9947,#9948,#9949,#9950,#9951,#9952,#9953,#9954,#9955,#9956,#9957,
#9958,#9959,#9960,#9961,#9962,#9963,#9964),.UNSPECIFIED.,.F.,.F.,(4,3,3,
3,3,3,3,3,3,3,3,3,4),(0.,0.053523079491772,0.107745541051727,0.117301531762597,
0.171497090450284,0.19946878868074,0.234298606923062,0.287998861062908,
0.34252758042597,0.351197710209308,0.408243668718811,0.4613343165756,0.465289627228313),
 .UNSPECIFIED.);
#208=B_SPLINE_CURVE_WITH_KNOTS('',3,(#9967,#9968,#9969,#9970,#9971,#9972,
#9973,#9974,#9975,#9976,#9977,#9978,#9979,#9980,#9981,#9982,#9983,#9984,
#9985,#9986,#9987,#9988,#9989,#9990,#9991,#9992,#9993,#9994),
 .UNSPECIFIED.,.F.,.F.,(4,3,3,3,3,3,3,3,3,4),(0.,0.0238139464176845,0.039101051769884,
0.0628789982206146,0.0664894862143964,0.0781003874493316,0.102014483019035,
0.11706667068295,0.140827139970411,0.155096347075245),.UNSPECIFIED.);
#209=B_SPLINE_CURVE_WITH_KNOTS('',3,(#9996,#9997,#9998,#9999),
 .UNSPECIFIED.,.F.,.F.,(4,4),(2.42791692093292E-5,0.602904494019558),
 .UNSPECIFIED.);
#210=B_SPLINE_CURVE_WITH_KNOTS('',3,(#10002,#10003,#10004,#10005),
 .UNSPECIFIED.,.F.,.F.,(4,4),(0.8033909285608,4.02187648095927),
 .UNSPECIFIED.);
#211=B_SPLINE_CURVE_WITH_KNOTS('',3,(#10008,#10009,#10010,#10011,#10012,
#10013,#10014,#10015,#10016,#10017),.UNSPECIFIED.,.F.,.F.,(4,3,3,4),(4.22337623295021,
6.17414866693447,6.32726315261627,8.45313487255185),.UNSPECIFIED.);
#212=B_SPLINE_CURVE_WITH_KNOTS('',3,(#10021,#10022,#10023,#10024),
 .UNSPECIFIED.,.F.,.F.,(4,4),(12.3921295467468,12.6843586902602),
 .UNSPECIFIED.);
#213=B_SPLINE_CURVE_WITH_KNOTS('',3,(#10026,#10027,#10028,#10029,#10030,
#10031,#10032,#10033,#10034,#10035,#10036,#10037,#10038,#10039,#10040,#10041,
#10042,#10043,#10044,#10045,#10046,#10047,#10048,#10049,#10050,#10051,#10052,
#10053,#10054,#10055,#10056,#10057,#10058,#10059),.UNSPECIFIED.,.F.,.F.,
(4,3,3,3,3,3,3,3,3,3,3,4),(0.,0.0238043957114055,0.0391346151758438,0.0629652053320384,
0.0721593756253901,0.0781571886687045,0.101948185591131,0.117123476992186,
0.12020682003633,0.142665945482357,0.166389927689249,0.168222194312373),
 .UNSPECIFIED.);
#214=B_SPLINE_CURVE_WITH_KNOTS('',3,(#10063,#10064,#10065,#10066,#10067,
#10068,#10069,#10070,#10071,#10072,#10073,#10074,#10075,#10076,#10077,#10078,
#10079,#10080,#10081,#10082,#10083,#10084,#10085,#10086,#10087,#10088,#10089,
#10090,#10091,#10092,#10093,#10094,#10095,#10096),.UNSPECIFIED.,.F.,.F.,
(4,3,3,3,3,3,3,3,3,3,3,4),(0.,0.023797882907907,0.039102479174454,0.0629340675289177,
0.0721439954475325,0.0781021576199648,0.101891255326939,0.117067721419617,
0.120193732390416,0.142636523050355,0.16636673084783,0.168220399847748),
 .UNSPECIFIED.);
#215=B_SPLINE_CURVE_WITH_KNOTS('',3,(#10098,#10099,#10100,#10101),
 .UNSPECIFIED.,.F.,.F.,(4,4),(2.71213177756024E-5,0.290725780256064),
 .UNSPECIFIED.);
#216=B_SPLINE_CURVE_WITH_KNOTS('',3,(#10111,#10112,#10113,#10114,#10115,
#10116),.UNSPECIFIED.,.F.,.F.,(4,2,4),(-0.6065913737563,-0.303324265158378,
-0.00121210420063977),.UNSPECIFIED.);
#217=B_SPLINE_CURVE_WITH_KNOTS('',3,(#10118,#10119,#10120,#10121,#10122,
#10123),.UNSPECIFIED.,.F.,.F.,(4,2,4),(-0.605468679705391,-0.303324901248498,
-8.9425867424664E-5),.UNSPECIFIED.);
#218=B_SPLINE_CURVE_WITH_KNOTS('',3,(#10125,#10126,#10127,#10128,#10129,
#10130,#10131,#10132,#10133,#10134,#10135,#10136,#10137,#10138,#10139,#10140,
#10141,#10142,#10143,#10144,#10145,#10146,#10147,#10148,#10149,#10150,#10151,
#10152),.UNSPECIFIED.,.F.,.F.,(4,3,3,3,3,3,3,3,3,4),(-0.153261590805415,
-0.129427422483982,-0.117093626371441,-0.093122524304512,-0.077863059046492,
-0.0655799937729104,-0.0417579003169496,-0.0388648221790391,-0.0150894148558222,
0.),.UNSPECIFIED.);
#219=B_SPLINE_CURVE_WITH_KNOTS('',3,(#10155,#10156,#10157,#10158,#10159,
#10160,#10161,#10162,#10163,#10164,#10165,#10166,#10167,#10168,#10169,#10170,
#10171,#10172,#10173,#10174,#10175,#10176,#10177,#10178,#10179,#10180,#10181,
#10182),.UNSPECIFIED.,.F.,.F.,(4,3,3,3,3,3,3,3,3,4),(-0.153296867786173,
-0.129546774976449,-0.118009772088948,-0.0941871764575653,-0.08771862273971,
-0.0788646444725944,-0.0549216410880561,-0.0394902966566095,-0.0156128557692252,
0.),.UNSPECIFIED.);
#220=B_SPLINE_CURVE_WITH_KNOTS('',3,(#10199,#10200,#10201,#10202),
 .UNSPECIFIED.,.F.,.F.,(4,4),(-4.3123055228435,-0.796205213256333),
 .UNSPECIFIED.);
#221=B_SPLINE_CURVE_WITH_KNOTS('',3,(#10220,#10221,#10222,#10223),
 .UNSPECIFIED.,.F.,.F.,(4,4),(-0.594853877716395,-0.335767855111383),
 .UNSPECIFIED.);
#222=B_SPLINE_CURVE_WITH_KNOTS('',3,(#10224,#10225,#10226,#10227),
 .UNSPECIFIED.,.F.,.F.,(4,4),(-0.615688454110788,-0.00935595183171186),
 .UNSPECIFIED.);
#223=B_SPLINE_CURVE_WITH_KNOTS('',3,(#10248,#10249,#10250,#10251),
 .UNSPECIFIED.,.F.,.F.,(4,4),(0.806548880270408,4.31873271634551),
 .UNSPECIFIED.);
#224=B_SPLINE_CURVE_WITH_KNOTS('',3,(#10273,#10274,#10275,#10276),
 .UNSPECIFIED.,.F.,.F.,(4,4),(0.335767855111383,0.605460332260614),
 .UNSPECIFIED.);
#225=B_SPLINE_CURVE_WITH_KNOTS('',3,(#10279,#10280,#10281,#10282),
 .UNSPECIFIED.,.F.,.F.,(4,4),(8.8675541747208,12.379738010796),
 .UNSPECIFIED.);
#226=B_SPLINE_CURVE_WITH_KNOTS('',3,(#10285,#10286,#10287,#10288),
 .UNSPECIFIED.,.F.,.F.,(4,4),(12.5808265588057,12.8505190359549),
 .UNSPECIFIED.);
#227=B_SPLINE_CURVE_WITH_KNOTS('',3,(#10310,#10311,#10312,#10313),
 .UNSPECIFIED.,.F.,.F.,(4,4),(-12.3900816778099,-8.87398136822274),
 .UNSPECIFIED.);
#228=B_SPLINE_CURVE_WITH_KNOTS('',3,(#10347,#10348,#10349,#10350),
 .UNSPECIFIED.,.F.,.F.,(4,4),(0.00935595183171174,0.615688454110787),
 .UNSPECIFIED.);
#229=B_SPLINE_CURVE_WITH_KNOTS('',3,(#10351,#10352,#10353,#10354),
 .UNSPECIFIED.,.F.,.F.,(4,4),(-12.8505190359549,-12.5914330133498),
 .UNSPECIFIED.);
#230=B_SPLINE_CURVE_WITH_KNOTS('',3,(#10357,#10358,#10359,#10360,#10361,
#10362),.UNSPECIFIED.,.F.,.F.,(4,2,4),(-0.606830654194234,-0.303665168982051,
-0.00091389508118378),.UNSPECIFIED.);
#231=B_SPLINE_CURVE_WITH_KNOTS('',3,(#10364,#10365,#10366,#10367,#10368,
#10369,#10370,#10371,#10372,#10373,#10374,#10375,#10376,#10377,#10378,#10379,
#10380,#10381,#10382,#10383,#10384,#10385,#10386,#10387,#10388,#10389,#10390,
#10391),.UNSPECIFIED.,.F.,.F.,(4,3,3,3,3,3,3,3,3,4),(-0.152562937837783,
-0.12881903955137,-0.117160811640917,-0.0932181166800446,-0.0780374575565173,
-0.0653603882662585,-0.0415602279441365,-0.0389951227734853,-0.0152093108541457,
0.),.UNSPECIFIED.);
#232=B_SPLINE_CURVE_WITH_KNOTS('',3,(#10395,#10396,#10397,#10398,#10399,
#10400,#10401,#10402,#10403,#10404,#10405,#10406,#10407,#10408,#10409,#10410,
#10411,#10412,#10413,#10414,#10415,#10416,#10417,#10418,#10419,#10420,#10421,
#10422),.UNSPECIFIED.,.F.,.F.,(4,3,3,3,3,3,3,3,3,4),(-0.152573286042523,
-0.128801685906155,-0.115487540236632,-0.091707628219999,-0.0872268515824704,
-0.07838422198738,-0.0544695788315335,-0.0392121213631617,-0.0154211067806385,
0.),.UNSPECIFIED.);
#233=B_SPLINE_CURVE_WITH_KNOTS('',3,(#10423,#10424,#10425,#10426,#10427,
#10428),.UNSPECIFIED.,.F.,.F.,(4,2,4),(-0.606417229744719,-0.30366508312326,
-0.000500462001714608),.UNSPECIFIED.);
#234=B_SPLINE_CURVE_WITH_KNOTS('',3,(#10445,#10446,#10447,#10448),
 .UNSPECIFIED.,.F.,.F.,(4,4),(-8.7204856127415,-4.5128966022766),
 .UNSPECIFIED.);
#235=B_SPLINE_CURVE_WITH_KNOTS('',3,(#10469,#10470,#10471,#10472),
 .UNSPECIFIED.,.F.,.F.,(4,4),(4.51913891174751,8.72381854299666),
 .UNSPECIFIED.);
#236=B_SPLINE_CURVE_WITH_KNOTS('',3,(#10474,#10475,#10476,#10477),
 .UNSPECIFIED.,.F.,.F.,(4,4),(4.46246834806959,8.66714797931881),
 .UNSPECIFIED.);
#237=B_SPLINE_CURVE_WITH_KNOTS('',3,(#10498,#10499,#10500,#10501),
 .UNSPECIFIED.,.F.,.F.,(4,4),(-8.67339028878965,-4.46580127832475),
 .UNSPECIFIED.);
#238=B_SPLINE_CURVE_WITH_KNOTS('',3,(#10520,#10521,#10522,#10523,#10524,
#10525),.UNSPECIFIED.,.F.,.F.,(4,2,4),(-0.607391644691745,-0.303762155877002,
-0.00125172564267001),.UNSPECIFIED.);
#239=B_SPLINE_CURVE_WITH_KNOTS('',3,(#10526,#10527,#10528,#10529,#10530,
#10531,#10532,#10533,#10534,#10535,#10536,#10537,#10538,#10539,#10540,#10541,
#10542,#10543,#10544,#10545,#10546,#10547,#10548,#10549,#10550,#10551,#10552,
#10553),.UNSPECIFIED.,.F.,.F.,(4,3,3,3,3,3,3,3,3,4),(-0.152281539067936,
-0.12854821222061,-0.115190816126163,-0.0912758856104041,-0.0781043161616985,
-0.0652713841318381,-0.0414808619979686,-0.039045740680325,-0.0152551599791835,
0.),.UNSPECIFIED.);
#240=B_SPLINE_CURVE_WITH_KNOTS('',3,(#10555,#10556,#10557,#10558,#10559,
#10560,#10561,#10562,#10563,#10564,#10565,#10566,#10567,#10568,#10569,#10570,
#10571,#10572,#10573,#10574,#10575,#10576,#10577,#10578,#10579,#10580,#10581,
#10582),.UNSPECIFIED.,.F.,.F.,(4,3,3,3,3,3,3,3,3,4),(-0.152284734818265,
-0.128510300097745,-0.115243636037359,-0.0914764658269932,-0.0870316758632336,
-0.078197793898112,-0.0542955901223581,-0.0391042908842167,-0.0153462458625635,
0.),.UNSPECIFIED.);
#241=B_SPLINE_CURVE_WITH_KNOTS('',3,(#10583,#10584,#10585,#10586,#10587,
#10588),.UNSPECIFIED.,.F.,.F.,(4,2,4),(-0.606273164239037,-0.303762187833104,
-0.000133245189939568),.UNSPECIFIED.);
#242=B_SPLINE_CURVE_WITH_KNOTS('',3,(#10605,#10606,#10607,#10608),
 .UNSPECIFIED.,.F.,.F.,(4,4),(-12.1227852464729,-8.92068531110742),
 .UNSPECIFIED.);
#243=B_SPLINE_CURVE_WITH_KNOTS('',3,(#10649,#10650,#10651,#10652),
 .UNSPECIFIED.,.F.,.F.,(4,4),(-4.26560157995882,-1.06350164459338),
 .UNSPECIFIED.);
#244=B_SPLINE_CURVE_WITH_KNOTS('',3,(#10671,#10672,#10673,#10674,#10675,
#10676),.UNSPECIFIED.,.F.,.F.,(4,2,4),(-0.607545900263938,-0.303784727094449,
-0.00134539382494125),.UNSPECIFIED.);
#245=B_SPLINE_CURVE_WITH_KNOTS('',3,(#10678,#10679,#10680,#10681,#10682,
#10683,#10684,#10685,#10686,#10687,#10688,#10689,#10690,#10691,#10692,#10693,
#10694,#10695,#10696,#10697,#10698,#10699,#10700,#10701,#10702,#10703,#10704,
#10705),.UNSPECIFIED.,.F.,.F.,(4,3,3,3,3,3,3,3,3,4),(-0.152214473108837,
-0.128485298747135,-0.115164309990209,-0.0912534321321267,-0.0781163092888813,
-0.0652482412471129,-0.0414606388666645,-0.0390548598067502,-0.0152611452145655,
0.),.UNSPECIFIED.);
#246=B_SPLINE_CURVE_WITH_KNOTS('',3,(#10709,#10710,#10711,#10712,#10713,
#10714,#10715,#10716,#10717,#10718,#10719,#10720,#10721,#10722,#10723,#10724,
#10725,#10726,#10727,#10728,#10729,#10730,#10731,#10732,#10733,#10734,#10735,
#10736),.UNSPECIFIED.,.F.,.F.,(4,3,3,3,3,3,3,3,3,4),(-0.152216110966007,
-0.128438825687404,-0.115191384846861,-0.0914281188167518,-0.0869870566155827,
-0.0781642271790374,-0.0542662950786889,-0.0390848818783988,-0.0153309789665,
0.),.UNSPECIFIED.);
#247=B_SPLINE_CURVE_WITH_KNOTS('',3,(#10737,#10738,#10739,#10740,#10741,
#10742),.UNSPECIFIED.,.F.,.F.,(4,2,4),(-0.606227037063105,-0.303784766192107,
-2.65251918123988E-5),.UNSPECIFIED.);
#248=B_SPLINE_CURVE_WITH_KNOTS('',3,(#10760,#10761,#10762,#10763),
 .UNSPECIFIED.,.F.,.F.,(4,4),(0.0107208554739345,0.617725317592517),
 .UNSPECIFIED.);
#249=B_SPLINE_CURVE_WITH_KNOTS('',3,(#10764,#10765,#10766,#10767),
 .UNSPECIFIED.,.F.,.F.,(4,4),(-12.893479658151,-12.3228618033436),
 .UNSPECIFIED.);
#250=B_SPLINE_CURVE_WITH_KNOTS('',3,(#10790,#10791,#10792,#10793),
 .UNSPECIFIED.,.F.,.F.,(4,4),(12.3251818525939,12.893479658151),
 .UNSPECIFIED.);
#251=B_SPLINE_CURVE_WITH_KNOTS('',3,(#10797,#10798,#10799,#10800),
 .UNSPECIFIED.,.F.,.F.,(4,4),(0.292807233425235,0.861105038472338),
 .UNSPECIFIED.);
#252=B_SPLINE_CURVE_WITH_KNOTS('',3,(#10818,#10819,#10820,#10821),
 .UNSPECIFIED.,.F.,.F.,(4,4),(-0.863425087722636,-0.29280723291527),
 .UNSPECIFIED.);
#253=B_SPLINE_CURVE_WITH_KNOTS('',3,(#10822,#10823,#10824,#10825),
 .UNSPECIFIED.,.F.,.F.,(4,4),(-0.617725317592517,-0.0107208554739345),
 .UNSPECIFIED.);
#254=B_SPLINE_CURVE_WITH_KNOTS('',3,(#10909,#10910,#10911,#10912),
 .UNSPECIFIED.,.F.,.F.,(4,4),(0.00878563933291533,0.615688454110788),
 .UNSPECIFIED.);
#255=B_SPLINE_CURVE_WITH_KNOTS('',3,(#10937,#10938,#10939,#10940),
 .UNSPECIFIED.,.F.,.F.,(4,4),(-0.615688454110787,-0.00878563933291527),
 .UNSPECIFIED.);
#256=B_SPLINE_CURVE_WITH_KNOTS('',3,(#11026,#11027,#11028,#11029),
 .UNSPECIFIED.,.F.,.F.,(4,4),(-9.62771529167128E-17,0.617725317592517),
 .UNSPECIFIED.);
#257=B_SPLINE_CURVE_WITH_KNOTS('',3,(#11030,#11031,#11032,#11033),
 .UNSPECIFIED.,.F.,.F.,(4,4),(-0.617725317592517,-0.000337488966422091),
 .UNSPECIFIED.);
#258=B_SPLINE_CURVE_WITH_KNOTS('',3,(#11069,#11070,#11071,#11072,#11073),
 .UNSPECIFIED.,.F.,.F.,(4,1,4),(-12.893479658151,-5.71764434212835,-0.335767855111383),
 .UNSPECIFIED.);
#259=B_SPLINE_CURVE_WITH_KNOTS('',3,(#11074,#11075,#11076,#11077,#11078),
 .UNSPECIFIED.,.F.,.F.,(4,1,4),(0.335767855111383,5.71764434212835,12.893479658151),
 .UNSPECIFIED.);
#260=B_SPLINE_CURVE_WITH_KNOTS('',3,(#11103,#11104,#11105,#11106),
 .UNSPECIFIED.,.F.,.F.,(4,4),(-0.00171041937131743,0.615688454110788),
 .UNSPECIFIED.);
#261=B_SPLINE_CURVE_WITH_KNOTS('',3,(#11107,#11108,#11109,#11110),
 .UNSPECIFIED.,.F.,.F.,(4,4),(-0.615688454110788,-3.98826847727851E-7),
 .UNSPECIFIED.);
#262=B_SPLINE_CURVE_WITH_KNOTS('',3,(#11135,#11136,#11137,#11138),
 .UNSPECIFIED.,.F.,.F.,(4,4),(3.98826847219577E-7,0.615688454110787),
 .UNSPECIFIED.);
#263=B_SPLINE_CURVE_WITH_KNOTS('',3,(#11139,#11140,#11141,#11142),
 .UNSPECIFIED.,.F.,.F.,(4,4),(-0.615688454110787,0.0017104193713176),
 .UNSPECIFIED.);
#264=B_SPLINE_CURVE_WITH_KNOTS('',3,(#11168,#11169,#11170,#11171,#11172),
 .UNSPECIFIED.,.F.,.F.,(4,1,4),(-12.8505190359549,-7.4686425489379,-0.29280723291527),
 .UNSPECIFIED.);
#265=B_SPLINE_CURVE_WITH_KNOTS('',3,(#11173,#11174,#11175,#11176,#11177),
 .UNSPECIFIED.,.F.,.F.,(4,1,4),(0.292807233425236,7.4686425489379,12.8505190359549),
 .UNSPECIFIED.);
#266=B_SPLINE_CURVE_WITH_KNOTS('',3,(#11198,#11199,#11200,#11201),
 .UNSPECIFIED.,.F.,.F.,(4,4),(0.000337488966421928,0.617725317592517),
 .UNSPECIFIED.);
#267=B_SPLINE_CURVE_WITH_KNOTS('',3,(#11202,#11203,#11204,#11205),
 .UNSPECIFIED.,.F.,.F.,(4,4),(-0.617725317592517,8.06646416329215E-17),
 .UNSPECIFIED.);
#268=B_SPLINE_CURVE_WITH_KNOTS('',3,(#11245,#11246,#11247,#11248),
 .UNSPECIFIED.,.F.,.F.,(4,4),(3.28016616408593,4.26236080300681),
 .UNSPECIFIED.);
#269=B_SPLINE_CURVE_WITH_KNOTS('',3,(#11252,#11253,#11254,#11255),
 .UNSPECIFIED.,.F.,.F.,(4,4),(8.92392608805945,9.90612072688831),
 .UNSPECIFIED.);
#270=B_SPLINE_CURVE_WITH_KNOTS('',3,(#11257,#11258,#11259,#11260,#11261,
#11262,#11263,#11264,#11265,#11266,#11267,#11268,#11269,#11270,#11271,#11272,
#11273,#11274,#11275),.UNSPECIFIED.,.F.,.F.,(4,3,3,3,3,3,4),(-0.050768112872884,
-0.0388528786649772,-0.0311058171716578,-0.0259830388669653,-0.0210744122964195,
-0.0143837148934404,0.),.UNSPECIFIED.);
#271=B_SPLINE_CURVE_WITH_KNOTS('',3,(#11277,#11278,#11279,#11280),
 .UNSPECIFIED.,.F.,.F.,(4,4),(9.9568018127159,12.1251256661408),
 .UNSPECIFIED.);
#272=B_SPLINE_CURVE_WITH_KNOTS('',3,(#11284,#11285,#11286,#11287),
 .UNSPECIFIED.,.F.,.F.,(4,4),(1.06116122492545,3.22948508825557),
 .UNSPECIFIED.);
#273=B_SPLINE_CURVE_WITH_KNOTS('',3,(#11288,#11289,#11290,#11291,#11292,
#11293,#11294,#11295,#11296,#11297,#11298,#11299,#11300,#11301,#11302,#11303,
#11304,#11305,#11306),.UNSPECIFIED.,.F.,.F.,(4,3,3,3,3,3,4),(-0.0507681129736439,
-0.0388528772897764,-0.0311058147321604,-0.0259830361493327,-0.0210744097201194,
-0.0143837130754026,-9.90506278315E-9),.UNSPECIFIED.);
#274=B_SPLINE_CURVE_WITH_KNOTS('',3,(#11514,#11515,#11516,#11517,#11518,
#11519),.UNSPECIFIED.,.F.,.F.,(4,2,4),(-0.605566356596631,-0.303329629920269,
-0.000148729590407126),.UNSPECIFIED.);
#275=B_SPLINE_CURVE_WITH_KNOTS('',3,(#11521,#11522,#11523,#11524,#11525,
#11526,#11527,#11528,#11529,#11530,#11531,#11532,#11533,#11534,#11535,#11536,
#11537,#11538,#11539,#11540,#11541,#11542,#11543,#11544,#11545,#11546,#11547,
#11548),.UNSPECIFIED.,.F.,.F.,(4,3,3,3,3,3,3,3,3,4),(-0.153210533292091,
-0.129383071834804,-0.117098895005168,-0.0931297672424715,-0.0778761857300216,
-0.065564095006876,-0.0417435583396367,-0.038874550231651,-0.0150983388519663,
0.),.UNSPECIFIED.);
#276=B_SPLINE_CURVE_WITH_KNOTS('',3,(#11552,#11553,#11554,#11555,#11556,
#11557,#11558,#11559,#11560,#11561,#11562,#11563,#11564,#11565,#11566,#11567,
#11568,#11569,#11570,#11571,#11572,#11573,#11574,#11575,#11576,#11577,#11578,
#11579),.UNSPECIFIED.,.F.,.F.,(4,3,3,3,3,3,3,3,3,4),(-0.153244081227051,
-0.129493605146206,-0.117970006482883,-0.0941492904140308,-0.0876825809854227,
-0.078828741443105,-0.0548877675055393,-0.0394694906046094,-0.0155984926894347,
0.),.UNSPECIFIED.);
#277=B_SPLINE_CURVE_WITH_KNOTS('',3,(#11580,#11581,#11582,#11583,#11584,
#11585),.UNSPECIFIED.,.F.,.F.,(4,2,4),(-0.606539490527658,-0.303329031627741,
-0.00112184825655631),.UNSPECIFIED.);
#278=B_SPLINE_CURVE_WITH_KNOTS('',3,(#11590,#11591,#11592,#11593,#11594,
#11595),.UNSPECIFIED.,.F.,.F.,(4,2,4),(-0.606785247764818,-0.303663188081886,
-0.00088649083675002),.UNSPECIFIED.);
#279=B_SPLINE_CURVE_WITH_KNOTS('',3,(#11597,#11598,#11599,#11600,#11601,
#11602,#11603,#11604,#11605,#11606,#11607,#11608,#11609,#11610,#11611,#11612,
#11613,#11614,#11615,#11616,#11617,#11618,#11619,#11620,#11621,#11622,#11623,
#11624),.UNSPECIFIED.,.F.,.F.,(4,3,3,3,3,3,3,3,3,4),(-0.15258577077829,
-0.128839317352572,-0.117158786685373,-0.0932148261566644,-0.0780319390000633,
-0.0653676349965338,-0.0415665498371782,-0.0389909618069961,-0.0152059030050533,
0.),.UNSPECIFIED.);
#280=B_SPLINE_CURVE_WITH_KNOTS('',3,(#11628,#11629,#11630,#11631,#11632,
#11633,#11634,#11635,#11636,#11637,#11638,#11639,#11640,#11641,#11642,#11643,
#11644,#11645,#11646,#11647,#11648,#11649,#11650,#11651,#11652,#11653,#11654,
#11655),.UNSPECIFIED.,.F.,.F.,(4,3,3,3,3,3,3,3,3,4),(-0.152596853546747,
-0.128825864440686,-0.115507515430042,-0.0917263797372463,-0.0872428123353572,
-0.0783995504057471,-0.0544835945915644,-0.0392209901554083,-0.0154275313391792,
0.),.UNSPECIFIED.);
#281=B_SPLINE_CURVE_WITH_KNOTS('',3,(#11657,#11658,#11659,#11660,#11661,
#11662),.UNSPECIFIED.,.F.,.F.,(4,2,4),(-0.606440835737524,-0.303663090452391,
-0.000542069086802599),.UNSPECIFIED.);
#282=B_SPLINE_CURVE_WITH_KNOTS('',3,(#11668,#11669,#11670,#11671,#11672,
#11673),.UNSPECIFIED.,.F.,.F.,(4,2,4),(-0.607379220946441,-0.303761646676304,
-0.00124422999587004),.UNSPECIFIED.);
#283=B_SPLINE_CURVE_WITH_KNOTS('',3,(#11675,#11676,#11677,#11678,#11679,
#11680,#11681,#11682,#11683,#11684,#11685,#11686,#11687,#11688,#11689,#11690,
#11691,#11692,#11693,#11694,#11695,#11696,#11697,#11698,#11699,#11700,#11701,
#11702),.UNSPECIFIED.,.F.,.F.,(4,3,3,3,3,3,3,3,3,4),(-0.152287640102895,
-0.128554450486317,-0.115193035178751,-0.0912770810520543,-0.0781028969167454,
-0.0652733399726575,-0.0414820896655672,-0.0390446621366508,-0.0152552334863041,
0.),.UNSPECIFIED.);
#284=B_SPLINE_CURVE_WITH_KNOTS('',3,(#11706,#11707,#11708,#11709,#11710,
#11711,#11712,#11713,#11714,#11715,#11716,#11717,#11718,#11719,#11720,#11721,
#11722,#11723,#11724,#11725,#11726,#11727,#11728,#11729,#11730,#11731,#11732,
#11733),.UNSPECIFIED.,.F.,.F.,(4,3,3,3,3,3,3,3,3,4),(-0.152291020205185,
-0.128517753946702,-0.115248901231919,-0.0914807886786037,-0.0870359119466785,
-0.0782017654295232,-0.054298407767766,-0.03910658747416,-0.0153486482327859,
0.),.UNSPECIFIED.);
#285=B_SPLINE_CURVE_WITH_KNOTS('',3,(#11735,#11736,#11737,#11738,#11739,
#11740),.UNSPECIFIED.,.F.,.F.,(4,2,4),(-0.606279550122448,-0.303761677523001,
-0.000144559171857295),.UNSPECIFIED.);
#286=B_SPLINE_CURVE_WITH_KNOTS('',3,(#11746,#11747,#11748,#11749,#11750,
#11751),.UNSPECIFIED.,.F.,.F.,(4,2,4),(-0.607536685592867,-0.303784463250135,
-0.00133982193348342),.UNSPECIFIED.);
#287=B_SPLINE_CURVE_WITH_KNOTS('',3,(#11752,#11753,#11754,#11755,#11756,
#11757,#11758,#11759,#11760,#11761,#11762,#11763,#11764,#11765,#11766,#11767,
#11768,#11769,#11770,#11771,#11772,#11773,#11774,#11775,#11776,#11777,#11778,
#11779),.UNSPECIFIED.,.F.,.F.,(4,3,3,3,3,3,3,3,3,4),(-0.152217684890348,
-0.128490376540845,-0.11516578527262,-0.091253137134092,-0.0781160865160423,
-0.0652495101170982,-0.0414606291875136,-0.0390546905501479,-0.015263466236765,
0.),.UNSPECIFIED.);
#288=B_SPLINE_CURVE_WITH_KNOTS('',3,(#11781,#11782,#11783,#11784,#11785,
#11786,#11787,#11788,#11789,#11790,#11791,#11792,#11793,#11794,#11795,#11796,
#11797,#11798,#11799,#11800,#11801,#11802,#11803,#11804,#11805,#11806,#11807,
#11808),.UNSPECIFIED.,.F.,.F.,(4,3,3,3,3,3,3,3,3,4),(-0.152219351639196,
-0.128444680332832,-0.115193337419806,-0.0914284185691762,-0.0869890032859244,
-0.0781648487722283,-0.0542647883944502,-0.0390852411900305,-0.0153331469286526,
0.),.UNSPECIFIED.);
#289=B_SPLINE_CURVE_WITH_KNOTS('',3,(#11810,#11811,#11812,#11813,#11814,
#11815),.UNSPECIFIED.,.F.,.F.,(4,2,4),(-0.606231877025315,-0.303784501204342,
-3.50089943914611E-5),.UNSPECIFIED.);
#290=B_SPLINE_CURVE_WITH_KNOTS('',3,(#11821,#11822,#11823,#11824),
 .UNSPECIFIED.,.F.,.F.,(4,4),(0.0108333608245492,0.617725317592517),
 .UNSPECIFIED.);
#291=B_SPLINE_CURVE_WITH_KNOTS('',3,(#11828,#11829,#11830,#11831),
 .UNSPECIFIED.,.F.,.F.,(4,4),(-0.617725317592517,-0.0108333608245492),
 .UNSPECIFIED.);
#292=B_SPLINE_CURVE_WITH_KNOTS('',3,(#11834,#11835,#11836,#11837),
 .UNSPECIFIED.,.F.,.F.,(4,4),(8.65483889175297,12.1899094612697),
 .UNSPECIFIED.);
#293=B_SPLINE_CURVE_WITH_KNOTS('',3,(#11838,#11839,#11840,#11841),
 .UNSPECIFIED.,.F.,.F.,(4,4),(0.491886782059505,4.00844302274363),
 .UNSPECIFIED.);
#294=B_SPLINE_CURVE_WITH_KNOTS('',3,(#11844,#11845,#11846,#11847,#11848,
#11849,#11850,#11851,#11852,#11853),.UNSPECIFIED.,.F.,.F.,(4,3,3,4),(4.20909064274042,
6.3236533433415,8.26419514194387,8.41669725637478),.UNSPECIFIED.);
#295=B_SPLINE_CURVE_WITH_KNOTS('',3,(#11856,#11857,#11858,#11859),
 .UNSPECIFIED.,.F.,.F.,(4,4),(8.61714174069208,11.8187712274298),
 .UNSPECIFIED.);
#296=B_SPLINE_CURVE_WITH_KNOTS('',3,(#11863,#11864,#11865,#11866),
 .UNSPECIFIED.,.F.,.F.,(4,4),(12.0182076143484,12.6179302061492),
 .UNSPECIFIED.);
#297=B_SPLINE_CURVE_WITH_KNOTS('',3,(#11867,#11868,#11869,#11870,#11871,
#11872,#11873,#11874,#11875,#11876,#11877,#11878,#11879,#11880,#11881,#11882,
#11883,#11884,#11885,#11886,#11887,#11888,#11889,#11890,#11891,#11892,#11893,
#11894),.UNSPECIFIED.,.F.,.F.,(4,3,3,3,3,3,3,3,3,4),(0.,0.023812730958415,
0.0390943730497349,0.0628727645281949,0.0664866407211859,0.0780895647789142,
0.102003044086093,0.117056568347941,0.14081843048439,0.155095961761698),
 .UNSPECIFIED.);
#298=B_SPLINE_CURVE_WITH_KNOTS('',3,(#11898,#11899,#11900,#11901,#11902,
#11903,#11904,#11905,#11906,#11907,#11908,#11909,#11910,#11911,#11912,#11913,
#11914,#11915,#11916,#11917,#11918,#11919,#11920,#11921,#11922,#11923,#11924,
#11925,#11926,#11927,#11928,#11929,#11930,#11931,#11932,#11933,#11934),
 .UNSPECIFIED.,.F.,.F.,(4,3,3,3,3,3,3,3,3,3,3,3,4),(0.,0.0535193130531386,
0.107740084455895,0.117281563739951,0.171478196787188,0.199460035548543,
0.234266327019636,0.287962832542679,0.34249270416273,0.351167719367162,
0.408228095477446,0.46132246935065,0.46528847158773),.UNSPECIFIED.);
#299=B_SPLINE_CURVE_WITH_KNOTS('',3,(#11936,#11937,#11938,#11939),
 .UNSPECIFIED.,.F.,.F.,(4,4),(0.0221781183199723,0.974834454777906),
 .UNSPECIFIED.);
#300=B_SPLINE_CURVE_WITH_KNOTS('',3,(#11941,#11942,#11943,#11944,#11945,
#11946,#11947,#11948,#11949,#11950,#11951,#11952,#11953,#11954,#11955,#11956,
#11957,#11958,#11959,#11960,#11961,#11962,#11963,#11964,#11965,#11966,#11967,
#11968,#11969,#11970,#11971,#11972,#11973,#11974,#11975,#11976,#11977,#11978,
#11979,#11980,#11981,#11982,#11983),.UNSPECIFIED.,.F.,.F.,(4,3,3,3,3,3,
3,3,3,3,3,3,3,3,4),(0.,0.0533317239385299,0.107762434368039,0.117305236535198,
0.171635266834242,0.216430402805854,0.234303130921432,0.288010415584935,
0.341932185058889,0.351200358601802,0.360578786332496,0.414653942238971,
0.427906071157934,0.482008506259547,0.504658879840573),.UNSPECIFIED.);
#301=B_SPLINE_CURVE_WITH_KNOTS('',3,(#11987,#11988,#11989,#11990,#11991,
#11992,#11993,#11994,#11995,#11996,#11997,#11998,#11999,#12000,#12001,#12002,
#12003,#12004,#12005,#12006,#12007,#12008,#12009,#12010,#12011,#12012,#12013,
#12014,#12015,#12016,#12017,#12018,#12019,#12020,#12021,#12022,#12023,#12024,
#12025,#12026,#12027,#12028,#12029),.UNSPECIFIED.,.F.,.F.,(4,3,3,3,3,3,
3,3,3,3,3,3,3,3,4),(0.,0.0533492049661439,0.107791770949794,0.117401360885473,
0.171729175646356,0.216477851539682,0.234467324023732,0.288191829779795,
0.342104640447882,0.351366010290958,0.360619117109406,0.414688080797906,
0.427993719046535,0.482081475021072,0.504664253934307),.UNSPECIFIED.);
#302=B_SPLINE_CURVE_WITH_KNOTS('',3,(#12031,#12032,#12033,#12034),
 .UNSPECIFIED.,.F.,.F.,(4,4),(0.0251655452220943,0.977821881680028),
 .UNSPECIFIED.);
#303=B_SPLINE_CURVE_WITH_KNOTS('',3,(#12036,#12037,#12038,#12039,#12040,
#12041,#12042,#12043,#12044,#12045,#12046,#12047,#12048,#12049,#12050,#12051,
#12052,#12053,#12054,#12055,#12056,#12057,#12058,#12059,#12060,#12061,#12062,
#12063,#12064,#12065,#12066,#12067,#12068,#12069,#12070,#12071,#12072),
 .UNSPECIFIED.,.F.,.F.,(4,3,3,3,3,3,3,3,3,3,3,3,4),(0.,0.053523079491772,
0.107745541051727,0.117301531762597,0.171497090450284,0.19946878868074,
0.234298606923062,0.287998861062908,0.34252758042597,0.351197710209308,
0.408243668718811,0.4613343165756,0.465289627228313),.UNSPECIFIED.);
#304=B_SPLINE_CURVE_WITH_KNOTS('',3,(#12075,#12076,#12077,#12078,#12079,
#12080,#12081,#12082,#12083,#12084,#12085,#12086,#12087,#12088,#12089,#12090,
#12091,#12092,#12093,#12094,#12095,#12096,#12097,#12098,#12099,#12100,#12101,
#12102),.UNSPECIFIED.,.F.,.F.,(4,3,3,3,3,3,3,3,3,4),(0.,0.0238139464176845,
0.039101051769884,0.0628789982206146,0.0664894862143964,0.0781003874493316,
0.102014483019035,0.11706667068295,0.140827139970411,0.155096347075245),
 .UNSPECIFIED.);
#305=B_SPLINE_CURVE_WITH_KNOTS('',3,(#12104,#12105,#12106,#12107),
 .UNSPECIFIED.,.F.,.F.,(4,4),(2.42791692093292E-5,0.602904494019558),
 .UNSPECIFIED.);
#306=B_SPLINE_CURVE_WITH_KNOTS('',3,(#12110,#12111,#12112,#12113),
 .UNSPECIFIED.,.F.,.F.,(4,4),(0.8033909285608,4.02187648095927),
 .UNSPECIFIED.);
#307=B_SPLINE_CURVE_WITH_KNOTS('',3,(#12116,#12117,#12118,#12119,#12120,
#12121,#12122,#12123,#12124,#12125),.UNSPECIFIED.,.F.,.F.,(4,3,3,4),(4.22337623295021,
6.17414866693447,6.32726315261627,8.45313487255185),.UNSPECIFIED.);
#308=B_SPLINE_CURVE_WITH_KNOTS('',3,(#12129,#12130,#12131,#12132),
 .UNSPECIFIED.,.F.,.F.,(4,4),(12.3921295467468,12.6843586902602),
 .UNSPECIFIED.);
#309=B_SPLINE_CURVE_WITH_KNOTS('',3,(#12134,#12135,#12136,#12137,#12138,
#12139,#12140,#12141,#12142,#12143,#12144,#12145,#12146,#12147,#12148,#12149,
#12150,#12151,#12152,#12153,#12154,#12155,#12156,#12157,#12158,#12159,#12160,
#12161,#12162,#12163,#12164,#12165,#12166,#12167),.UNSPECIFIED.,.F.,.F.,
(4,3,3,3,3,3,3,3,3,3,3,4),(0.,0.0238043957114055,0.0391346151758438,0.0629652053320384,
0.0721593756253901,0.0781571886687045,0.101948185591131,0.117123476992186,
0.12020682003633,0.142665945482357,0.166389927689249,0.168222194312373),
 .UNSPECIFIED.);
#310=B_SPLINE_CURVE_WITH_KNOTS('',3,(#12171,#12172,#12173,#12174,#12175,
#12176,#12177,#12178,#12179,#12180,#12181,#12182,#12183,#12184,#12185,#12186,
#12187,#12188,#12189,#12190,#12191,#12192,#12193,#12194,#12195,#12196,#12197,
#12198,#12199,#12200,#12201,#12202,#12203,#12204),.UNSPECIFIED.,.F.,.F.,
(4,3,3,3,3,3,3,3,3,3,3,4),(0.,0.023797882907907,0.039102479174454,0.0629340675289177,
0.0721439954475325,0.0781021576199648,0.101891255326939,0.117067721419617,
0.120193732390416,0.142636523050355,0.16636673084783,0.168220399847748),
 .UNSPECIFIED.);
#311=B_SPLINE_CURVE_WITH_KNOTS('',3,(#12206,#12207,#12208,#12209),
 .UNSPECIFIED.,.F.,.F.,(4,4),(2.71213177756024E-5,0.290725780256064),
 .UNSPECIFIED.);
#312=B_SPLINE_CURVE_WITH_KNOTS('',3,(#12219,#12220,#12221,#12222,#12223,
#12224),.UNSPECIFIED.,.F.,.F.,(4,2,4),(-0.6065913737563,-0.303324265158378,
-0.00121210420063977),.UNSPECIFIED.);
#313=B_SPLINE_CURVE_WITH_KNOTS('',3,(#12226,#12227,#12228,#12229,#12230,
#12231),.UNSPECIFIED.,.F.,.F.,(4,2,4),(-0.605468679705391,-0.303324901248498,
-8.9425867424664E-5),.UNSPECIFIED.);
#314=B_SPLINE_CURVE_WITH_KNOTS('',3,(#12233,#12234,#12235,#12236,#12237,
#12238,#12239,#12240,#12241,#12242,#12243,#12244,#12245,#12246,#12247,#12248,
#12249,#12250,#12251,#12252,#12253,#12254,#12255,#12256,#12257,#12258,#12259,
#12260),.UNSPECIFIED.,.F.,.F.,(4,3,3,3,3,3,3,3,3,4),(-0.153261590805415,
-0.129427422483982,-0.117093626371441,-0.093122524304512,-0.077863059046492,
-0.0655799937729104,-0.0417579003169496,-0.0388648221790391,-0.0150894148558222,
0.),.UNSPECIFIED.);
#315=B_SPLINE_CURVE_WITH_KNOTS('',3,(#12263,#12264,#12265,#12266,#12267,
#12268,#12269,#12270,#12271,#12272,#12273,#12274,#12275,#12276,#12277,#12278,
#12279,#12280,#12281,#12282,#12283,#12284,#12285,#12286,#12287,#12288,#12289,
#12290),.UNSPECIFIED.,.F.,.F.,(4,3,3,3,3,3,3,3,3,4),(-0.153296867786173,
-0.129546774976449,-0.118009772088948,-0.0941871764575653,-0.08771862273971,
-0.0788646444725944,-0.0549216410880561,-0.0394902966566095,-0.0156128557692252,
0.),.UNSPECIFIED.);
#316=B_SPLINE_CURVE_WITH_KNOTS('',3,(#12307,#12308,#12309,#12310),
 .UNSPECIFIED.,.F.,.F.,(4,4),(-4.3123055228435,-0.796205213256333),
 .UNSPECIFIED.);
#317=B_SPLINE_CURVE_WITH_KNOTS('',3,(#12328,#12329,#12330,#12331),
 .UNSPECIFIED.,.F.,.F.,(4,4),(-0.594853877716395,-0.335767855111383),
 .UNSPECIFIED.);
#318=B_SPLINE_CURVE_WITH_KNOTS('',3,(#12332,#12333,#12334,#12335),
 .UNSPECIFIED.,.F.,.F.,(4,4),(-0.615688454110788,-0.00935595183171186),
 .UNSPECIFIED.);
#319=B_SPLINE_CURVE_WITH_KNOTS('',3,(#12356,#12357,#12358,#12359),
 .UNSPECIFIED.,.F.,.F.,(4,4),(0.806548880270408,4.31873271634551),
 .UNSPECIFIED.);
#320=B_SPLINE_CURVE_WITH_KNOTS('',3,(#12381,#12382,#12383,#12384),
 .UNSPECIFIED.,.F.,.F.,(4,4),(0.335767855111383,0.605460332260614),
 .UNSPECIFIED.);
#321=B_SPLINE_CURVE_WITH_KNOTS('',3,(#12387,#12388,#12389,#12390),
 .UNSPECIFIED.,.F.,.F.,(4,4),(8.8675541747208,12.379738010796),
 .UNSPECIFIED.);
#322=B_SPLINE_CURVE_WITH_KNOTS('',3,(#12393,#12394,#12395,#12396),
 .UNSPECIFIED.,.F.,.F.,(4,4),(12.5808265588057,12.8505190359549),
 .UNSPECIFIED.);
#323=B_SPLINE_CURVE_WITH_KNOTS('',3,(#12418,#12419,#12420,#12421),
 .UNSPECIFIED.,.F.,.F.,(4,4),(-12.3900816778099,-8.87398136822274),
 .UNSPECIFIED.);
#324=B_SPLINE_CURVE_WITH_KNOTS('',3,(#12455,#12456,#12457,#12458),
 .UNSPECIFIED.,.F.,.F.,(4,4),(0.00935595183171174,0.615688454110787),
 .UNSPECIFIED.);
#325=B_SPLINE_CURVE_WITH_KNOTS('',3,(#12459,#12460,#12461,#12462),
 .UNSPECIFIED.,.F.,.F.,(4,4),(-12.8505190359549,-12.5914330133498),
 .UNSPECIFIED.);
#326=B_SPLINE_CURVE_WITH_KNOTS('',3,(#12465,#12466,#12467,#12468,#12469,
#12470),.UNSPECIFIED.,.F.,.F.,(4,2,4),(-0.606830654194234,-0.303665168982051,
-0.00091389508118378),.UNSPECIFIED.);
#327=B_SPLINE_CURVE_WITH_KNOTS('',3,(#12472,#12473,#12474,#12475,#12476,
#12477,#12478,#12479,#12480,#12481,#12482,#12483,#12484,#12485,#12486,#12487,
#12488,#12489,#12490,#12491,#12492,#12493,#12494,#12495,#12496,#12497,#12498,
#12499),.UNSPECIFIED.,.F.,.F.,(4,3,3,3,3,3,3,3,3,4),(-0.152562937837783,
-0.12881903955137,-0.117160811640917,-0.0932181166800446,-0.0780374575565173,
-0.0653603882662585,-0.0415602279441365,-0.0389951227734853,-0.0152093108541457,
0.),.UNSPECIFIED.);
#328=B_SPLINE_CURVE_WITH_KNOTS('',3,(#12503,#12504,#12505,#12506,#12507,
#12508,#12509,#12510,#12511,#12512,#12513,#12514,#12515,#12516,#12517,#12518,
#12519,#12520,#12521,#12522,#12523,#12524,#12525,#12526,#12527,#12528,#12529,
#12530),.UNSPECIFIED.,.F.,.F.,(4,3,3,3,3,3,3,3,3,4),(-0.152573286042523,
-0.128801685906155,-0.115487540236632,-0.091707628219999,-0.0872268515824704,
-0.07838422198738,-0.0544695788315335,-0.0392121213631617,-0.0154211067806385,
0.),.UNSPECIFIED.);
#329=B_SPLINE_CURVE_WITH_KNOTS('',3,(#12531,#12532,#12533,#12534,#12535,
#12536),.UNSPECIFIED.,.F.,.F.,(4,2,4),(-0.606417229744719,-0.30366508312326,
-0.000500462001714608),.UNSPECIFIED.);
#330=B_SPLINE_CURVE_WITH_KNOTS('',3,(#12553,#12554,#12555,#12556),
 .UNSPECIFIED.,.F.,.F.,(4,4),(-8.7204856127415,-4.5128966022766),
 .UNSPECIFIED.);
#331=B_SPLINE_CURVE_WITH_KNOTS('',3,(#12577,#12578,#12579,#12580),
 .UNSPECIFIED.,.F.,.F.,(4,4),(4.51913891174751,8.72381854299666),
 .UNSPECIFIED.);
#332=B_SPLINE_CURVE_WITH_KNOTS('',3,(#12582,#12583,#12584,#12585),
 .UNSPECIFIED.,.F.,.F.,(4,4),(4.46246834806959,8.66714797931881),
 .UNSPECIFIED.);
#333=B_SPLINE_CURVE_WITH_KNOTS('',3,(#12606,#12607,#12608,#12609),
 .UNSPECIFIED.,.F.,.F.,(4,4),(-8.67339028878965,-4.46580127832475),
 .UNSPECIFIED.);
#334=B_SPLINE_CURVE_WITH_KNOTS('',3,(#12628,#12629,#12630,#12631,#12632,
#12633),.UNSPECIFIED.,.F.,.F.,(4,2,4),(-0.607391644691745,-0.303762155877002,
-0.00125172564267001),.UNSPECIFIED.);
#335=B_SPLINE_CURVE_WITH_KNOTS('',3,(#12634,#12635,#12636,#12637,#12638,
#12639,#12640,#12641,#12642,#12643,#12644,#12645,#12646,#12647,#12648,#12649,
#12650,#12651,#12652,#12653,#12654,#12655,#12656,#12657,#12658,#12659,#12660,
#12661),.UNSPECIFIED.,.F.,.F.,(4,3,3,3,3,3,3,3,3,4),(-0.152281539067936,
-0.12854821222061,-0.115190816126163,-0.0912758856104041,-0.0781043161616985,
-0.0652713841318381,-0.0414808619979686,-0.039045740680325,-0.0152551599791835,
0.),.UNSPECIFIED.);
#336=B_SPLINE_CURVE_WITH_KNOTS('',3,(#12663,#12664,#12665,#12666,#12667,
#12668,#12669,#12670,#12671,#12672,#12673,#12674,#12675,#12676,#12677,#12678,
#12679,#12680,#12681,#12682,#12683,#12684,#12685,#12686,#12687,#12688,#12689,
#12690),.UNSPECIFIED.,.F.,.F.,(4,3,3,3,3,3,3,3,3,4),(-0.152284734818265,
-0.128510300097745,-0.115243636037359,-0.0914764658269932,-0.0870316758632336,
-0.078197793898112,-0.0542955901223581,-0.0391042908842167,-0.0153462458625635,
0.),.UNSPECIFIED.);
#337=B_SPLINE_CURVE_WITH_KNOTS('',3,(#12691,#12692,#12693,#12694,#12695,
#12696),.UNSPECIFIED.,.F.,.F.,(4,2,4),(-0.606273164239037,-0.303762187833104,
-0.000133245189939568),.UNSPECIFIED.);
#338=B_SPLINE_CURVE_WITH_KNOTS('',3,(#12713,#12714,#12715,#12716),
 .UNSPECIFIED.,.F.,.F.,(4,4),(-12.1227852464729,-8.92068531110742),
 .UNSPECIFIED.);
#339=B_SPLINE_CURVE_WITH_KNOTS('',3,(#12757,#12758,#12759,#12760),
 .UNSPECIFIED.,.F.,.F.,(4,4),(-4.26560157995882,-1.06350164459338),
 .UNSPECIFIED.);
#340=B_SPLINE_CURVE_WITH_KNOTS('',3,(#12779,#12780,#12781,#12782,#12783,
#12784),.UNSPECIFIED.,.F.,.F.,(4,2,4),(-0.607545900263938,-0.303784727094449,
-0.00134539382494125),.UNSPECIFIED.);
#341=B_SPLINE_CURVE_WITH_KNOTS('',3,(#12786,#12787,#12788,#12789,#12790,
#12791,#12792,#12793,#12794,#12795,#12796,#12797,#12798,#12799,#12800,#12801,
#12802,#12803,#12804,#12805,#12806,#12807,#12808,#12809,#12810,#12811,#12812,
#12813),.UNSPECIFIED.,.F.,.F.,(4,3,3,3,3,3,3,3,3,4),(-0.152214473108837,
-0.128485298747135,-0.115164309990209,-0.0912534321321267,-0.0781163092888813,
-0.0652482412471129,-0.0414606388666645,-0.0390548598067502,-0.0152611452145655,
0.),.UNSPECIFIED.);
#342=B_SPLINE_CURVE_WITH_KNOTS('',3,(#12817,#12818,#12819,#12820,#12821,
#12822,#12823,#12824,#12825,#12826,#12827,#12828,#12829,#12830,#12831,#12832,
#12833,#12834,#12835,#12836,#12837,#12838,#12839,#12840,#12841,#12842,#12843,
#12844),.UNSPECIFIED.,.F.,.F.,(4,3,3,3,3,3,3,3,3,4),(-0.152216110966007,
-0.128438825687404,-0.115191384846861,-0.0914281188167518,-0.0869870566155827,
-0.0781642271790374,-0.0542662950786889,-0.0390848818783988,-0.0153309789665,
0.),.UNSPECIFIED.);
#343=B_SPLINE_CURVE_WITH_KNOTS('',3,(#12845,#12846,#12847,#12848,#12849,
#12850),.UNSPECIFIED.,.F.,.F.,(4,2,4),(-0.606227037063105,-0.303784766192107,
-2.65251918123988E-5),.UNSPECIFIED.);
#344=B_SPLINE_CURVE_WITH_KNOTS('',3,(#12868,#12869,#12870,#12871),
 .UNSPECIFIED.,.F.,.F.,(4,4),(0.0107208554739345,0.617725317592517),
 .UNSPECIFIED.);
#345=B_SPLINE_CURVE_WITH_KNOTS('',3,(#12872,#12873,#12874,#12875),
 .UNSPECIFIED.,.F.,.F.,(4,4),(-12.893479658151,-12.3228618033436),
 .UNSPECIFIED.);
#346=B_SPLINE_CURVE_WITH_KNOTS('',3,(#12898,#12899,#12900,#12901),
 .UNSPECIFIED.,.F.,.F.,(4,4),(12.3251818525939,12.893479658151),
 .UNSPECIFIED.);
#347=B_SPLINE_CURVE_WITH_KNOTS('',3,(#12905,#12906,#12907,#12908),
 .UNSPECIFIED.,.F.,.F.,(4,4),(0.292807233425235,0.861105038472338),
 .UNSPECIFIED.);
#348=B_SPLINE_CURVE_WITH_KNOTS('',3,(#12926,#12927,#12928,#12929),
 .UNSPECIFIED.,.F.,.F.,(4,4),(-0.863425087722636,-0.29280723291527),
 .UNSPECIFIED.);
#349=B_SPLINE_CURVE_WITH_KNOTS('',3,(#12930,#12931,#12932,#12933),
 .UNSPECIFIED.,.F.,.F.,(4,4),(-0.617725317592517,-0.0107208554739345),
 .UNSPECIFIED.);
#350=B_SPLINE_CURVE_WITH_KNOTS('',3,(#13017,#13018,#13019,#13020),
 .UNSPECIFIED.,.F.,.F.,(4,4),(0.00878563933291533,0.615688454110788),
 .UNSPECIFIED.);
#351=B_SPLINE_CURVE_WITH_KNOTS('',3,(#13045,#13046,#13047,#13048),
 .UNSPECIFIED.,.F.,.F.,(4,4),(-0.615688454110787,-0.00878563933291527),
 .UNSPECIFIED.);
#352=B_SPLINE_CURVE_WITH_KNOTS('',3,(#13134,#13135,#13136,#13137),
 .UNSPECIFIED.,.F.,.F.,(4,4),(-9.62771529167128E-17,0.617725317592517),
 .UNSPECIFIED.);
#353=B_SPLINE_CURVE_WITH_KNOTS('',3,(#13138,#13139,#13140,#13141),
 .UNSPECIFIED.,.F.,.F.,(4,4),(-0.617725317592517,-0.000337488966422091),
 .UNSPECIFIED.);
#354=B_SPLINE_CURVE_WITH_KNOTS('',3,(#13177,#13178,#13179,#13180,#13181),
 .UNSPECIFIED.,.F.,.F.,(4,1,4),(-12.893479658151,-5.71764434212835,-0.335767855111383),
 .UNSPECIFIED.);
#355=B_SPLINE_CURVE_WITH_KNOTS('',3,(#13182,#13183,#13184,#13185,#13186),
 .UNSPECIFIED.,.F.,.F.,(4,1,4),(0.335767855111383,5.71764434212835,12.893479658151),
 .UNSPECIFIED.);
#356=B_SPLINE_CURVE_WITH_KNOTS('',3,(#13211,#13212,#13213,#13214),
 .UNSPECIFIED.,.F.,.F.,(4,4),(-0.00171041937131743,0.615688454110788),
 .UNSPECIFIED.);
#357=B_SPLINE_CURVE_WITH_KNOTS('',3,(#13215,#13216,#13217,#13218),
 .UNSPECIFIED.,.F.,.F.,(4,4),(-0.615688454110788,-3.98826847727851E-7),
 .UNSPECIFIED.);
#358=B_SPLINE_CURVE_WITH_KNOTS('',3,(#13243,#13244,#13245,#13246),
 .UNSPECIFIED.,.F.,.F.,(4,4),(3.98826847219577E-7,0.615688454110787),
 .UNSPECIFIED.);
#359=B_SPLINE_CURVE_WITH_KNOTS('',3,(#13247,#13248,#13249,#13250),
 .UNSPECIFIED.,.F.,.F.,(4,4),(-0.615688454110787,0.0017104193713176),
 .UNSPECIFIED.);
#360=B_SPLINE_CURVE_WITH_KNOTS('',3,(#13276,#13277,#13278,#13279,#13280),
 .UNSPECIFIED.,.F.,.F.,(4,1,4),(-12.8505190359549,-7.4686425489379,-0.29280723291527),
 .UNSPECIFIED.);
#361=B_SPLINE_CURVE_WITH_KNOTS('',3,(#13281,#13282,#13283,#13284,#13285),
 .UNSPECIFIED.,.F.,.F.,(4,1,4),(0.292807233425236,7.4686425489379,12.8505190359549),
 .UNSPECIFIED.);
#362=B_SPLINE_CURVE_WITH_KNOTS('',3,(#13306,#13307,#13308,#13309),
 .UNSPECIFIED.,.F.,.F.,(4,4),(0.000337488966421928,0.617725317592517),
 .UNSPECIFIED.);
#363=B_SPLINE_CURVE_WITH_KNOTS('',3,(#13310,#13311,#13312,#13313),
 .UNSPECIFIED.,.F.,.F.,(4,4),(-0.617725317592517,8.06646416329215E-17),
 .UNSPECIFIED.);
#364=B_SPLINE_CURVE_WITH_KNOTS('',3,(#13447,#13448,#13449,#13450,#13451),
 .UNSPECIFIED.,.F.,.F.,(4,1,4),(-0.118017359897249,-0.0505788685273923,
0.),.UNSPECIFIED.);
#365=B_SPLINE_CURVE_WITH_KNOTS('',3,(#13454,#13455,#13456,#13457,#13458),
 .UNSPECIFIED.,.F.,.F.,(4,1,4),(0.,0.0505788685273923,0.118017359897249),
 .UNSPECIFIED.);
#366=B_SPLINE_CURVE_WITH_KNOTS('',3,(#13493,#13494,#13495,#13496,#13497),
 .UNSPECIFIED.,.F.,.F.,(4,1,4),(-0.118017359898262,-0.0505788685278266,
0.),.UNSPECIFIED.);
#367=B_SPLINE_CURVE_WITH_KNOTS('',3,(#13498,#13499,#13500,#13501,#13502),
 .UNSPECIFIED.,.F.,.F.,(4,1,4),(0.,0.0505788685278266,0.118017359898262),
 .UNSPECIFIED.);
#368=B_SPLINE_CURVE_WITH_KNOTS('',3,(#13531,#13532,#13533,#13534,#13535),
 .UNSPECIFIED.,.F.,.F.,(4,1,4),(-12.2100728150593,-5.23288834931112,0.),
 .UNSPECIFIED.);
#369=B_SPLINE_CURVE_WITH_KNOTS('',3,(#13536,#13537,#13538,#13539,#13540),
 .UNSPECIFIED.,.F.,.F.,(4,1,4),(0.,5.23288834931112,12.2100728150593),
 .UNSPECIFIED.);
#370=B_SPLINE_CURVE_WITH_KNOTS('',3,(#13569,#13570,#13571,#13572,#13573),
 .UNSPECIFIED.,.F.,.F.,(4,1,4),(-0.108129892237767,-0.0463413823988794,
-1.97133828064127E-11),.UNSPECIFIED.);
#371=B_SPLINE_CURVE_WITH_KNOTS('',3,(#13574,#13575,#13576,#13577,#13578),
 .UNSPECIFIED.,.F.,.F.,(4,1,4),(1.97133828064127E-11,0.0463413823988794,
0.108129892237767),.UNSPECIFIED.);
#372=B_SPLINE_CURVE_WITH_KNOTS('',3,(#13613,#13614,#13615,#13616,#13617),
 .UNSPECIFIED.,.F.,.F.,(4,1,4),(-0.108129892206815,-0.0463413823743492,
0.),.UNSPECIFIED.);
#373=B_SPLINE_CURVE_WITH_KNOTS('',3,(#13618,#13619,#13620,#13621,#13622),
 .UNSPECIFIED.,.F.,.F.,(4,1,4),(0.,0.0463413823743492,0.108129892206815),
 .UNSPECIFIED.);
#374=B_SPLINE_CURVE_WITH_KNOTS('',3,(#13648,#13649,#13650,#13651,#13652),
 .UNSPECIFIED.,.F.,.F.,(4,1,4),(-12.2100734167563,-6.97718480957529,-6.51086303075479E-13),
 .UNSPECIFIED.);
#375=B_SPLINE_CURVE_WITH_KNOTS('',3,(#13653,#13654,#13655,#13656,#13657),
 .UNSPECIFIED.,.F.,.F.,(4,1,4),(6.51086303075479E-13,6.97718480957529,12.2100734167563),
 .UNSPECIFIED.);
#376=B_SPLINE_CURVE_WITH_KNOTS('',3,(#13660,#13661,#13662,#13663),
 .UNSPECIFIED.,.F.,.F.,(4,4),(0.000181689894813921,0.124708996845866),
 .UNSPECIFIED.);
#377=B_SPLINE_CURVE_WITH_KNOTS('',3,(#13666,#13667,#13668,#13669),
 .UNSPECIFIED.,.F.,.F.,(4,4),(-0.124708996851356,-0.000181689894814102),
 .UNSPECIFIED.);
#378=B_SPLINE_CURVE_WITH_KNOTS('',3,(#13691,#13692,#13693,#13694),
 .UNSPECIFIED.,.F.,.F.,(4,4),(-0.124624122980966,-1.27068494615301E-16),
 .UNSPECIFIED.);
#379=B_SPLINE_CURVE_WITH_KNOTS('',3,(#13695,#13696,#13697,#13698,#13699,
#13700,#13701,#13702,#13703,#13704,#13705,#13706,#13707,#13708,#13709,#13710,
#13711,#13712,#13713,#13714,#13715,#13716,#13717,#13718,#13719,#13720,#13721,
#13722),.UNSPECIFIED.,.F.,.F.,(4,3,3,3,3,3,3,3,3,4),(0.,0.0322747504276753,
0.0586406101183928,0.090870813631105,0.0996503787243826,0.117132790114159,
0.149546322800321,0.175583390425035,0.207787925145658,0.232457773984835),
 .UNSPECIFIED.);
#380=B_SPLINE_CURVE_WITH_KNOTS('',3,(#13740,#13741,#13742,#13743),
 .UNSPECIFIED.,.F.,.F.,(4,4),(6.28713621962651E-9,0.124025126494243),
 .UNSPECIFIED.);
#381=B_SPLINE_CURVE_WITH_KNOTS('',3,(#13744,#13745,#13746,#13747),
 .UNSPECIFIED.,.F.,.F.,(4,4),(0.0116899650356219,0.986620910196183),
 .UNSPECIFIED.);
#382=B_SPLINE_CURVE_WITH_KNOTS('',3,(#13773,#13774,#13775,#13776),
 .UNSPECIFIED.,.F.,.F.,(4,4),(-0.12358375933533,0.000944809985246663),
 .UNSPECIFIED.);
#383=B_SPLINE_CURVE_WITH_KNOTS('',3,(#13777,#13778,#13779,#13780,#13781,
#13782,#13783,#13784,#13785,#13786,#13787,#13788,#13789,#13790,#13791,#13792,
#13793,#13794,#13795,#13796,#13797,#13798,#13799,#13800,#13801,#13802,#13803,
#13804,#13805,#13806,#13807,#13808,#13809,#13810),.UNSPECIFIED.,.F.,.F.,
(4,3,3,3,3,3,3,3,3,3,3,4),(0.,0.0322568536241053,0.0586526138523664,0.0909514856947606,
0.108742407475907,0.117151788463556,0.149394351344039,0.175600627102286,
0.181167420983902,0.214570374458228,0.246736309066329,0.253563811229603),
 .UNSPECIFIED.);
#384=B_SPLINE_CURVE_WITH_KNOTS('',3,(#13814,#13815,#13816,#13817),
 .UNSPECIFIED.,.F.,.F.,(4,4),(-0.000944809985246617,0.123583759335329),
 .UNSPECIFIED.);
#385=B_SPLINE_CURVE_WITH_KNOTS('',3,(#13840,#13841,#13842,#13843,#13844,
#13845,#13846,#13847,#13848,#13849,#13850,#13851,#13852,#13853,#13854,#13855,
#13856,#13857,#13858,#13859,#13860,#13861,#13862,#13863,#13864,#13865,#13866,
#13867),.UNSPECIFIED.,.F.,.F.,(4,3,3,3,3,3,3,3,3,4),(0.,0.0322765438584903,
0.0586513922310012,0.0908809480268686,0.099655003871439,0.117150238497558,
0.149564657711791,0.175599638586681,0.20780211537115,0.232458396023953),
 .UNSPECIFIED.);
#386=B_SPLINE_CURVE_WITH_KNOTS('',3,(#13868,#13869,#13870,#13871),
 .UNSPECIFIED.,.F.,.F.,(4,4),(3.30031141304588E-16,0.124624122970512),
 .UNSPECIFIED.);
#387=B_SPLINE_CURVE_WITH_KNOTS('',3,(#13897,#13898,#13899,#13900),
 .UNSPECIFIED.,.F.,.F.,(4,4),(-0.12402512649425,-6.28713634712869E-9),
 .UNSPECIFIED.);
#388=B_SPLINE_CURVE_WITH_KNOTS('',3,(#13901,#13902,#13903,#13904,#13905,
#13906,#13907,#13908,#13909,#13910,#13911,#13912,#13913,#13914,#13915,#13916,
#13917,#13918,#13919,#13920,#13921,#13922,#13923,#13924,#13925,#13926,#13927,
#13928,#13929,#13930,#13931,#13932,#13933,#13934),.UNSPECIFIED.,.F.,.F.,
(4,3,3,3,3,3,3,3,3,3,3,4),(0.,0.0322666769662355,0.0587055335553437,0.0910029078093924,
0.108768157423115,0.117242626226166,0.149488313345073,0.175692943342501,
0.181189289804584,0.214619150478997,0.24677571115805,0.253566775541772),
 .UNSPECIFIED.);
#389=B_SPLINE_CURVE_WITH_KNOTS('',3,(#13936,#13937,#13938,#13939),
 .UNSPECIFIED.,.F.,.F.,(4,4),(0.0133790898038168,0.988310034964378),
 .UNSPECIFIED.);
#390=B_SPLINE_CURVE_WITH_KNOTS('',3,(#13962,#13963,#13964,#13965,#13966,
#13967,#13968,#13969,#13970,#13971),.UNSPECIFIED.,.F.,.F.,(4,3,3,4),(-4.09202352044852,
-3.99057144343763,-2.99292858257822,-2.07317267331971),.UNSPECIFIED.);
#391=B_SPLINE_CURVE_WITH_KNOTS('',3,(#13974,#13975,#13976,#13977,#13978,
#13979,#13980),.UNSPECIFIED.,.F.,.F.,(4,3,4),(0.,0.998042281124014,1.12274180646116),
 .UNSPECIFIED.);
#392=B_SPLINE_CURVE_WITH_KNOTS('',3,(#13985,#13986,#13987,#13988,#13989,
#13990,#13991,#13992,#13993,#13994,#13995,#13996,#13997,#13998,#13999,#14000,
#14001,#14002,#14003,#14004,#14005,#14006),.UNSPECIFIED.,.F.,.F.,(4,3,3,
3,3,3,3,4),(-10.3752088276281,-9.97642860859406,-8.97878574773466,-7.98114288687525,
-6.98350002601584,-5.98585716515644,-4.98821430429703,-4.09202352044852),
 .UNSPECIFIED.);
#393=B_SPLINE_CURVE_WITH_KNOTS('',3,(#14007,#14008,#14009,#14010,#14011,
#14012,#14013,#14014,#14015,#14016,#14017,#14018,#14019,#14020,#14021,#14022,
#14023,#14024,#14025,#14026,#14027,#14028),.UNSPECIFIED.,.F.,.F.,(4,3,3,
3,3,3,3,4),(1.12274180646116,1.99608456224804,2.99412684337208,3.99216912449611,
4.99021140562014,5.98825368674417,6.98629596786821,7.40592711364074),
 .UNSPECIFIED.);
#394=B_SPLINE_CURVE_WITH_KNOTS('',3,(#14033,#14034,#14035,#14036,#14037,
#14038,#14039,#14040,#14041,#14042,#14043,#14044,#14045,#14046,#14047,#14048,
#14049,#14050,#14051,#14052,#14053,#14054),.UNSPECIFIED.,.F.,.F.,(4,3,3,
3,3,3,3,4),(-16.6583941348077,-15.9622857737505,-14.9646429128911,-13.9670000520317,
-12.9693571911723,-11.9717143303129,-10.9740714694535,-10.3752088276281),
 .UNSPECIFIED.);
#395=B_SPLINE_CURVE_WITH_KNOTS('',3,(#14055,#14056,#14057,#14058,#14059,
#14060,#14061,#14062,#14063,#14064,#14065,#14066,#14067,#14068,#14069,#14070,
#14071,#14072,#14073,#14074,#14075,#14076),.UNSPECIFIED.,.F.,.F.,(4,3,3,
3,3,3,3,4),(7.40592711364074,7.98433824899223,8.98238053011626,9.98042281124028,
10.9784650923643,11.9765073734883,12.9745496546124,13.6891124208203),
 .UNSPECIFIED.);
#396=B_SPLINE_CURVE_WITH_KNOTS('',3,(#14081,#14082,#14083,#14084,#14085,
#14086,#14087,#14088,#14089,#14090,#14091,#14092,#14093,#14094,#14095,#14096,
#14097,#14098,#14099,#14100,#14101,#14102),.UNSPECIFIED.,.F.,.F.,(4,3,3,
3,3,3,3,4),(-22.9415794419873,-21.9481429389069,-20.9505000780475,-19.9528572171881,
-18.9552143563287,-17.9575714954693,-16.9599286346099,-16.6583941348077),
 .UNSPECIFIED.);
#397=B_SPLINE_CURVE_WITH_KNOTS('',3,(#14103,#14104,#14105,#14106,#14107,
#14108,#14109,#14110,#14111,#14112,#14113,#14114,#14115,#14116,#14117,#14118,
#14119,#14120,#14121,#14122,#14123,#14124,#14125,#14126,#14127),
 .UNSPECIFIED.,.F.,.F.,(4,3,3,3,3,3,3,3,4),(13.6891124208203,13.9725919357364,
14.9706342168604,15.9686764979844,16.9667187791085,17.9647610602325,18.9628033413565,
19.9608456224805,19.9722977279999),.UNSPECIFIED.);
#398=B_SPLINE_CURVE_WITH_KNOTS('',3,(#14132,#14133,#14134,#14135,#14136,
#14137,#14138,#14139,#14140,#14141,#14142,#14143,#14144,#14145,#14146,#14147,
#14148,#14149,#14150,#14151,#14152,#14153),.UNSPECIFIED.,.F.,.F.,(4,3,3,
3,3,3,3,4),(-29.2247647491669,-28.9316429649228,-27.9340001040634,-26.936357243204,
-25.9387143823446,-24.9410715214852,-23.9434286606257,-22.9415794419873),
 .UNSPECIFIED.);
#399=B_SPLINE_CURVE_WITH_KNOTS('',3,(#14154,#14155,#14156,#14157,#14158,
#14159,#14160,#14161,#14162,#14163,#14164,#14165,#14166,#14167,#14168,#14169,
#14170,#14171,#14172,#14173,#14174,#14175),.UNSPECIFIED.,.F.,.F.,(4,3,3,
3,3,3,3,4),(19.9722977279999,20.9588879036046,21.9569301847286,22.9549724658526,
23.9530147469767,24.9510570281007,25.9490993092247,26.2554830351795),
 .UNSPECIFIED.);
#400=B_SPLINE_CURVE_WITH_KNOTS('',3,(#14180,#14181,#14182,#14183,#14184,
#14185,#14186,#14187,#14188,#14189,#14190,#14191,#14192,#14193,#14194,#14195,
#14196,#14197,#14198,#14199,#14200,#14201),.UNSPECIFIED.,.F.,.F.,(4,3,3,
3,3,3,3,4),(-35.5079500563465,-34.9175001300792,-33.9198572692198,-32.9222144083604,
-31.924571547501,-30.9269286866416,-29.9292858257822,-29.2247647491669),
 .UNSPECIFIED.);
#401=B_SPLINE_CURVE_WITH_KNOTS('',3,(#14202,#14203,#14204,#14205,#14206,
#14207,#14208,#14209,#14210,#14211,#14212,#14213,#14214,#14215,#14216,#14217,
#14218,#14219,#14220,#14221,#14222,#14223),.UNSPECIFIED.,.F.,.F.,(4,3,3,
3,3,3,3,4),(26.2554830351795,26.9471415903487,27.9451838714728,28.9432261525968,
29.9412684337208,30.9393107148448,31.9373529959689,32.5386683423591),
 .UNSPECIFIED.);
#402=B_SPLINE_CURVE_WITH_KNOTS('',3,(#14228,#14229,#14230,#14231,#14232,
#14233,#14234,#14235,#14236,#14237,#14238,#14239,#14240,#14241,#14242,#14243,
#14244,#14245,#14246,#14247,#14248,#14249),.UNSPECIFIED.,.F.,.F.,(4,3,3,
3,3,3,3,4),(-41.791135363526,-40.9033572952357,-39.9057144343762,-38.9080715735168,
-37.9104287126574,-36.912785851798,-35.9151429909386,-35.5079500563465),
 .UNSPECIFIED.);
#403=B_SPLINE_CURVE_WITH_KNOTS('',3,(#14250,#14251,#14252,#14253,#14254,
#14255,#14256,#14257,#14258,#14259,#14260,#14261,#14262,#14263,#14264,#14265,
#14266,#14267,#14268,#14269,#14270,#14271),.UNSPECIFIED.,.F.,.F.,(4,3,3,
3,3,3,3,4),(32.5386683423591,32.9353952770929,33.9334375582169,34.931479839341,
35.929522120465,36.927564401589,37.9256066827131,38.8218536495387),
 .UNSPECIFIED.);
#404=B_SPLINE_CURVE_WITH_KNOTS('',3,(#14276,#14277,#14278,#14279,#14280,
#14281,#14282,#14283,#14284,#14285,#14286,#14287,#14288,#14289,#14290,#14291,
#14292,#14293,#14294,#14295,#14296,#14297,#14298,#14299,#14300),
 .UNSPECIFIED.,.F.,.F.,(4,3,3,3,3,3,3,3,4),(-48.0743206707056,-47.8868573212515,
-46.8892144603921,-45.8915715995327,-44.8939287386733,-43.8962858778139,
-42.8986430169545,-41.9010001560951,-41.791135363526),.UNSPECIFIED.);
#405=B_SPLINE_CURVE_WITH_KNOTS('',3,(#14301,#14302,#14303,#14304,#14305,
#14306,#14307,#14308,#14309,#14310,#14311,#14312,#14313,#14314,#14315,#14316,
#14317,#14318,#14319,#14320,#14321,#14322,#14323,#14324,#14325),
 .UNSPECIFIED.,.F.,.F.,(4,3,3,3,3,3,3,3,4),(38.8218536495387,38.9236489638371,
39.9216912449611,40.9197335260851,41.9177758072091,42.9158180883332,43.9138603694572,
44.9119026505812,45.1050389567183),.UNSPECIFIED.);
#406=B_SPLINE_CURVE_WITH_KNOTS('',3,(#14330,#14331,#14332,#14333,#14334,
#14335,#14336,#14337,#14338,#14339,#14340,#14341,#14342,#14343,#14344,#14345,
#14346,#14347,#14348,#14349,#14350,#14351),.UNSPECIFIED.,.F.,.F.,(4,3,3,
3,3,3,3,4),(-54.3575059778852,-53.8727144864079,-52.8750716255485,-51.8774287646891,
-50.8797859038297,-49.8821430429703,-48.8845001821109,-48.0743206707056),
 .UNSPECIFIED.);
#407=B_SPLINE_CURVE_WITH_KNOTS('',3,(#14352,#14353,#14354,#14355,#14356,
#14357,#14358,#14359,#14360,#14361,#14362,#14363,#14364,#14365,#14366,#14367,
#14368,#14369,#14370,#14371,#14372,#14373),.UNSPECIFIED.,.F.,.F.,(4,3,3,
3,3,3,3,4),(45.1050389567183,45.9099449317052,46.9079872128293,47.9060294939533,
48.9040717750773,49.9021140562014,50.9001563373254,51.3882242638979),
 .UNSPECIFIED.);
#408=B_SPLINE_CURVE_WITH_KNOTS('',3,(#14378,#14379,#14380,#14381,#14382,
#14383,#14384,#14385,#14386,#14387,#14388,#14389,#14390,#14391,#14392,#14393,
#14394,#14395,#14396,#14397,#14398,#14399),.UNSPECIFIED.,.F.,.F.,(4,3,3,
3,3,3,3,4),(-60.6406912850648,-59.8585716515644,-58.860928790705,-57.8632859298455,
-56.8656430689861,-55.8680002081267,-54.8703573472673,-54.3575059778852),
 .UNSPECIFIED.);
#409=B_SPLINE_CURVE_WITH_KNOTS('',3,(#14400,#14401,#14402,#14403,#14404,
#14405,#14406,#14407,#14408,#14409,#14410,#14411,#14412,#14413,#14414,#14415,
#14416,#14417,#14418,#14419,#14420,#14421),.UNSPECIFIED.,.F.,.F.,(4,3,3,
3,3,3,3,4),(51.3882242638979,51.8981986184494,52.8962408995734,53.8942831806975,
54.8923254618215,55.8903677429455,56.8884100240695,57.6714095710775),
 .UNSPECIFIED.);
#410=B_SPLINE_CURVE_WITH_KNOTS('',3,(#14426,#14427,#14428,#14429,#14430,
#14431,#14432,#14433,#14434,#14435,#14436,#14437,#14438,#14439,#14440,#14441,
#14442,#14443,#14444,#14445,#14446,#14447,#14448,#14449,#14450),
 .UNSPECIFIED.,.F.,.F.,(4,3,3,3,3,3,3,3,4),(-66.9238765922444,-66.8420716775802,
-65.8444288167208,-64.8467859558614,-63.849143095002,-62.8515002341426,
-61.8538573732832,-60.8562145124238,-60.6406912850648),.UNSPECIFIED.);
#411=B_SPLINE_CURVE_WITH_KNOTS('',3,(#14451,#14452,#14453,#14454,#14455,
#14456,#14457,#14458,#14459,#14460,#14461,#14462,#14463,#14464,#14465,#14466,
#14467,#14468,#14469,#14470,#14471,#14472,#14473,#14474,#14475),
 .UNSPECIFIED.,.F.,.F.,(4,3,3,3,3,3,3,3,4),(57.6714095710775,57.8864523051936,
58.8844945863176,59.8825368674416,60.8805791485657,61.8786214296897,62.8766637108137,
63.8747059919378,63.9545948782571),.UNSPECIFIED.);
#412=B_SPLINE_CURVE_WITH_KNOTS('',3,(#14480,#14481,#14482,#14483,#14484,
#14485,#14486,#14487,#14488,#14489,#14490,#14491,#14492,#14493,#14494,#14495,
#14496,#14497,#14498,#14499,#14500,#14501),.UNSPECIFIED.,.F.,.F.,(4,3,3,
3,3,3,3,4),(-73.207061899424,-72.8279288427366,-71.8302859818773,-70.8326431210178,
-69.8350002601584,-68.837357399299,-67.8397145384396,-66.9238765922444),
 .UNSPECIFIED.);
#413=B_SPLINE_CURVE_WITH_KNOTS('',3,(#14502,#14503,#14504,#14505,#14506,
#14507,#14508,#14509,#14510,#14511,#14512,#14513,#14514,#14515,#14516,#14517,
#14518,#14519,#14520,#14521,#14522,#14523),.UNSPECIFIED.,.F.,.F.,(4,3,3,
3,3,3,3,4),(63.9545948782571,64.8727482730618,65.8707905541858,66.8688328353098,
67.8668751164338,68.8649173975579,69.8629596786819,70.2377801854366),
 .UNSPECIFIED.);
#414=B_SPLINE_CURVE_WITH_KNOTS('',3,(#14528,#14529,#14530,#14531,#14532,
#14533,#14534,#14535,#14536,#14537,#14538,#14539,#14540,#14541,#14542,#14543,
#14544,#14545,#14546,#14547,#14548,#14549),.UNSPECIFIED.,.F.,.F.,(4,3,3,
3,3,3,3,4),(-79.4902472066036,-78.8137860078931,-77.8161431470337,-76.8185002861743,
-75.8208574253149,-74.8232145644555,-73.825571703596,-73.207061899424),
 .UNSPECIFIED.);
#415=B_SPLINE_CURVE_WITH_KNOTS('',3,(#14550,#14551,#14552,#14553,#14554,
#14555,#14556,#14557,#14558,#14559,#14560,#14561,#14562,#14563,#14564,#14565,
#14566,#14567,#14568,#14569,#14570,#14571),.UNSPECIFIED.,.F.,.F.,(4,3,3,
3,3,3,3,4),(70.2377801854366,70.8610019598059,71.85904424093,72.857086522054,
73.855128803178,74.853171084302,75.8512133654261,76.5209654926162),
 .UNSPECIFIED.);
#416=B_SPLINE_CURVE_WITH_KNOTS('',3,(#14576,#14577,#14578,#14579,#14580,
#14581,#14582,#14583,#14584,#14585,#14586,#14587,#14588,#14589,#14590,#14591,
#14592,#14593,#14594,#14595,#14596,#14597),.UNSPECIFIED.,.F.,.F.,(4,3,3,
3,3,3,3,4),(-85.7734325137832,-84.7996431730495,-83.8020003121901,-82.8043574513307,
-81.8067145904713,-80.8090717296119,-79.8114288687525,-79.4902472066036),
 .UNSPECIFIED.);
#417=B_SPLINE_CURVE_WITH_KNOTS('',3,(#14598,#14599,#14600,#14601,#14602,
#14603,#14604,#14605,#14606,#14607,#14608,#14609,#14610,#14611,#14612,#14613,
#14614,#14615,#14616,#14617,#14618,#14619),.UNSPECIFIED.,.F.,.F.,(4,3,3,
3,3,3,3,4),(76.5209654926162,76.8492556465501,77.8472979276741,78.8453402087982,
79.8433824899222,80.8414247710462,81.8394670521702,82.8041507997958),
 .UNSPECIFIED.);
#418=B_SPLINE_CURVE_WITH_KNOTS('',3,(#14624,#14625,#14626,#14627,#14628,
#14629,#14630,#14631,#14632,#14633,#14634,#14635,#14636,#14637,#14638,#14639,
#14640,#14641,#14642,#14643,#14644,#14645,#14646,#14647,#14648),
 .UNSPECIFIED.,.F.,.F.,(4,3,3,3,3,3,3,3,4),(-92.0566178209628,-91.7831431990654,
-90.7855003382059,-89.7878574773465,-88.7902146164871,-87.7925717556277,
-86.7949288947683,-85.7972860339089,-85.7734325137832),.UNSPECIFIED.);
#419=B_SPLINE_CURVE_WITH_KNOTS('',3,(#14649,#14650,#14651,#14652,#14653,
#14654,#14655,#14656,#14657,#14658,#14659,#14660,#14661,#14662,#14663,#14664,
#14665,#14666,#14667,#14668,#14669,#14670,#14671,#14672,#14673),
 .UNSPECIFIED.,.F.,.F.,(4,3,3,3,3,3,3,3,4),(82.8041507997958,82.8375093332942,
83.8355516144183,84.8335938955423,85.8316361766664,86.8296784577904,87.8277207389144,
88.8257630200384,89.0873361069754),.UNSPECIFIED.);
#420=B_SPLINE_CURVE_WITH_KNOTS('',3,(#14678,#14679,#14680,#14681,#14682,
#14683,#14684,#14685,#14686,#14687,#14688,#14689,#14690,#14691,#14692,#14693,
#14694,#14695,#14696,#14697,#14698,#14699),.UNSPECIFIED.,.F.,.F.,(4,3,3,
3,3,3,3,4),(-98.3398031281424,-97.7690003642218,-96.7713575033624,-95.773714642503,
-94.7760717816436,-93.7784289207842,-92.7807860599248,-92.0566178209628),
 .UNSPECIFIED.);
#421=B_SPLINE_CURVE_WITH_KNOTS('',3,(#14700,#14701,#14702,#14703,#14704,
#14705,#14706,#14707,#14708,#14709,#14710,#14711,#14712,#14713,#14714,#14715,
#14716,#14717,#14718,#14719,#14720,#14721),.UNSPECIFIED.,.F.,.F.,(4,3,3,
3,3,3,3,4),(89.0873361069754,89.8238053011624,90.8218475822865,91.8198898634105,
92.8179321445345,93.8159744256585,94.8140167067826,95.370521414155),
 .UNSPECIFIED.);
#422=B_SPLINE_CURVE_WITH_KNOTS('',3,(#14726,#14727,#14728,#14729,#14730,
#14731,#14732,#14733,#14734,#14735,#14736,#14737,#14738,#14739,#14740,#14741,
#14742,#14743,#14744,#14745,#14746,#14747),.UNSPECIFIED.,.F.,.F.,(4,3,3,
3,3,3,3,4),(-104.622988435322,-103.754857529378,-102.757214668519,-101.759571807659,
-100.7619289468,-99.7642860859406,-98.7666432250812,-98.3398031281424),
 .UNSPECIFIED.);
#423=B_SPLINE_CURVE_WITH_KNOTS('',3,(#14748,#14749,#14750,#14751,#14752,
#14753,#14754,#14755,#14756,#14757,#14758,#14759,#14760,#14761,#14762,#14763,
#14764,#14765,#14766,#14767,#14768,#14769),.UNSPECIFIED.,.F.,.F.,(4,3,3,
3,3,3,3,4),(95.370521414155,95.8120589879066,96.8101012690306,97.8081435501546,
98.8061858312787,99.8042281124027,100.802270393527,101.653706721335),
 .UNSPECIFIED.);
#424=B_SPLINE_CURVE_WITH_KNOTS('',3,(#14774,#14775,#14776,#14777,#14778,
#14779,#14780,#14781,#14782,#14783,#14784,#14785,#14786,#14787,#14788,#14789,
#14790,#14791,#14792,#14793,#14794,#14795,#14796,#14797,#14798),
 .UNSPECIFIED.,.F.,.F.,(4,3,3,3,3,3,3,3,4),(-110.906173742502,-110.738357555394,
-109.740714694535,-108.743071833675,-107.745428972816,-106.747786111956,
-105.750143251097,-104.752500390238,-104.622988435322),.UNSPECIFIED.);
#425=B_SPLINE_CURVE_WITH_KNOTS('',3,(#14799,#14800,#14801,#14802,#14803,
#14804,#14805,#14806,#14807,#14808,#14809,#14810,#14811,#14812,#14813,#14814,
#14815,#14816,#14817,#14818,#14819,#14820,#14821,#14822,#14823),
 .UNSPECIFIED.,.F.,.F.,(4,3,3,3,3,3,3,3,4),(101.653706721335,101.800312674651,
102.798354955775,103.796397236899,104.794439518023,105.792481799147,106.790524080271,
107.788566361395,107.936892028514),.UNSPECIFIED.);
#426=B_SPLINE_CURVE_WITH_KNOTS('',3,(#14828,#14829,#14830,#14831,#14832,
#14833,#14834,#14835,#14836,#14837,#14838,#14839,#14840,#14841,#14842,#14843,
#14844,#14845,#14846,#14847,#14848,#14849),.UNSPECIFIED.,.F.,.F.,(4,3,3,
3,3,3,3,4),(-117.189359049681,-116.724214720551,-115.726571859691,-114.728928998832,
-113.731286137972,-112.733643277113,-111.736000416253,-110.906173742502),
 .UNSPECIFIED.);
#427=B_SPLINE_CURVE_WITH_KNOTS('',3,(#14850,#14851,#14852,#14853,#14854,
#14855,#14856,#14857,#14858,#14859,#14860,#14861,#14862,#14863,#14864,#14865,
#14866,#14867,#14868,#14869,#14870,#14871),.UNSPECIFIED.,.F.,.F.,(4,3,3,
3,3,3,3,4),(107.936892028514,108.786608642519,109.784650923643,110.782693204767,
111.780735485891,112.778777767015,113.776820048139,114.220077335694),
 .UNSPECIFIED.);
#428=B_SPLINE_CURVE_WITH_KNOTS('',3,(#14876,#14877,#14878,#14879,#14880,
#14881,#14882,#14883,#14884,#14885,#14886,#14887,#14888,#14889,#14890,#14891,
#14892,#14893,#14894,#14895,#14896,#14897),.UNSPECIFIED.,.F.,.F.,(4,3,3,
3,3,3,3,4),(-123.472544356861,-122.710071885707,-121.712429024848,-120.714786163988,
-119.717143303129,-118.719500442269,-117.72185758141,-117.189359049681),
 .UNSPECIFIED.);
#429=B_SPLINE_CURVE_WITH_KNOTS('',3,(#14898,#14899,#14900,#14901,#14902,
#14903,#14904,#14905,#14906,#14907,#14908,#14909,#14910,#14911,#14912,#14913,
#14914,#14915,#14916,#14917,#14918,#14919),.UNSPECIFIED.,.F.,.F.,(4,3,3,
3,3,3,3,4),(114.220077335694,114.774862329263,115.772904610387,116.770946891511,
117.768989172635,118.767031453759,119.765073734883,120.503262642873),
 .UNSPECIFIED.);
#430=B_SPLINE_CURVE_WITH_KNOTS('',3,(#14924,#14925,#14926,#14927,#14928,
#14929,#14930,#14931,#14932,#14933,#14934,#14935,#14936,#14937,#14938,#14939,
#14940,#14941,#14942,#14943,#14944,#14945,#14946,#14947,#14948),
 .UNSPECIFIED.,.F.,.F.,(4,3,3,3,3,3,3,3,4),(-129.75572966404,-129.693571911723,
-128.695929050863,-127.698286190004,-126.700643329145,-125.703000468285,
-124.705357607426,-123.707714746566,-123.472544356861),.UNSPECIFIED.);
#431=B_SPLINE_CURVE_WITH_KNOTS('',3,(#14949,#14950,#14951,#14952,#14953,
#14954,#14955,#14956,#14957,#14958,#14959,#14960,#14961,#14962,#14963,#14964,
#14965,#14966,#14967,#14968,#14969,#14970,#14971,#14972,#14973),
 .UNSPECIFIED.,.F.,.F.,(4,3,3,3,3,3,3,3,4),(120.503262642873,120.763116016007,
121.761158297131,122.759200578255,123.757242859379,124.755285140503,125.753327421627,
126.751369702751,126.786447950053),.UNSPECIFIED.);
#432=B_SPLINE_CURVE_WITH_KNOTS('',3,(#14978,#14979,#14980,#14981,#14982,
#14983,#14984,#14985,#14986,#14987,#14988,#14989,#14990,#14991,#14992,#14993,
#14994,#14995,#14996,#14997,#14998,#14999),.UNSPECIFIED.,.F.,.F.,(4,3,3,
3,3,3,3,4),(-136.03891497122,-135.679429076879,-134.68178621602,-133.68414335516,
-132.686500494301,-131.688857633442,-130.691214772582,-129.75572966404),
 .UNSPECIFIED.);
#433=B_SPLINE_CURVE_WITH_KNOTS('',3,(#15000,#15001,#15002,#15003,#15004,
#15005,#15006,#15007,#15008,#15009,#15010,#15011,#15012,#15013,#15014,#15015,
#15016,#15017,#15018,#15019,#15020,#15021),.UNSPECIFIED.,.F.,.F.,(4,3,3,
3,3,3,3,4),(126.786447950053,127.749411983875,128.747454265,129.745496546124,
130.743538827248,131.741581108372,132.739623389496,133.069633257233),
 .UNSPECIFIED.);
#434=B_SPLINE_CURVE_WITH_KNOTS('',3,(#15026,#15027,#15028,#15029,#15030,
#15031,#15032,#15033,#15034,#15035,#15036,#15037,#15038,#15039,#15040,#15041,
#15042,#15043,#15044,#15045,#15046,#15047),.UNSPECIFIED.,.F.,.F.,(4,3,3,
3,3,3,3,4),(-142.322100278399,-141.665286242036,-140.667643381176,-139.670000520317,
-138.672357659457,-137.674714798598,-136.677071937739,-136.03891497122),
 .UNSPECIFIED.);
#435=B_SPLINE_CURVE_WITH_KNOTS('',3,(#15048,#15049,#15050,#15051,#15052,
#15053,#15054,#15055,#15056,#15057,#15058,#15059,#15060,#15061,#15062,#15063,
#15064,#15065,#15066,#15067,#15068,#15069),.UNSPECIFIED.,.F.,.F.,(4,3,3,
3,3,3,3,4),(133.069633257233,133.73766567062,134.735707951744,135.733750232868,
136.731792513992,137.729834795116,138.72787707624,139.352818564412),
 .UNSPECIFIED.);
#436=B_SPLINE_CURVE_WITH_KNOTS('',3,(#15074,#15075,#15076,#15077,#15078,
#15079,#15080,#15081,#15082,#15083,#15084,#15085,#15086,#15087,#15088,#15089,
#15090,#15091,#15092,#15093,#15094,#15095),.UNSPECIFIED.,.F.,.F.,(4,3,3,
3,3,3,3,4),(-148.605285585579,-147.651143407192,-146.653500546333,-145.655857685473,
-144.658214824614,-143.660571963754,-142.662929102895,-142.322100278399),
 .UNSPECIFIED.);
#437=B_SPLINE_CURVE_WITH_KNOTS('',3,(#15096,#15097,#15098,#15099,#15100,
#15101,#15102,#15103,#15104,#15105,#15106,#15107,#15108,#15109,#15110,#15111,
#15112,#15113,#15114,#15115,#15116,#15117),.UNSPECIFIED.,.F.,.F.,(4,3,3,
3,3,3,3,4),(139.352818564412,139.725919357364,140.723961638488,141.722003919612,
142.720046200736,143.71808848186,144.716130762984,145.636003871592),
 .UNSPECIFIED.);
#438=B_SPLINE_CURVE_WITH_KNOTS('',3,(#15122,#15123,#15124,#15125,#15126,
#15127,#15128,#15129,#15130,#15131,#15132,#15133,#15134,#15135,#15136,#15137,
#15138,#15139,#15140,#15141,#15142,#15143,#15144,#15145,#15146),
 .UNSPECIFIED.,.F.,.F.,(4,3,3,3,3,3,3,3,4),(-154.888470892759,-154.634643433208,
-153.637000572349,-152.639357711489,-151.64171485063,-150.64407198977,-149.646429128911,
-148.648786268052,-148.605285585579),.UNSPECIFIED.);
#439=B_SPLINE_CURVE_WITH_KNOTS('',3,(#15147,#15148,#15149,#15150,#15151,
#15152,#15153,#15154,#15155,#15156,#15157,#15158,#15159,#15160,#15161,#15162,
#15163,#15164,#15165,#15166,#15167,#15168,#15169,#15170,#15171),
 .UNSPECIFIED.,.F.,.F.,(4,3,3,3,3,3,3,3,4),(145.636003871592,145.714173044108,
146.712215325232,147.710257606356,148.70829988748,149.706342168604,150.704384449728,
151.702426730852,151.919189178771),.UNSPECIFIED.);
#440=B_SPLINE_CURVE_WITH_KNOTS('',3,(#15176,#15177,#15178,#15179,#15180,
#15181,#15182,#15183,#15184,#15185,#15186,#15187,#15188,#15189,#15190,#15191,
#15192,#15193,#15194,#15195,#15196,#15197),.UNSPECIFIED.,.F.,.F.,(4,3,3,
3,3,3,3,4),(-161.171656199938,-160.620500598364,-159.622857737505,-158.625214876646,
-157.627572015786,-156.629929154927,-155.632286294067,-154.888470892759),
 .UNSPECIFIED.);
#441=B_SPLINE_CURVE_WITH_KNOTS('',3,(#15198,#15199,#15200,#15201,#15202,
#15203,#15204,#15205,#15206,#15207,#15208,#15209,#15210,#15211,#15212,#15213,
#15214,#15215,#15216,#15217,#15218,#15219),.UNSPECIFIED.,.F.,.F.,(4,3,3,
3,3,3,3,4),(151.919189178771,152.700469011976,153.6985112931,154.696553574224,
155.694595855348,156.692638136472,157.690680417596,158.202374485951),
 .UNSPECIFIED.);
#442=B_SPLINE_CURVE_WITH_KNOTS('',3,(#15224,#15225,#15226,#15227,#15228,
#15229,#15230,#15231,#15232,#15233,#15234,#15235,#15236,#15237,#15238,#15239,
#15240,#15241,#15242,#15243,#15244,#15245),.UNSPECIFIED.,.F.,.F.,(4,3,3,
3,3,3,3,4),(-167.454841507118,-166.606357763521,-165.608714902661,-164.611072041802,
-163.613429180943,-162.615786320083,-161.618143459224,-161.171656199938),
 .UNSPECIFIED.);
#443=B_SPLINE_CURVE_WITH_KNOTS('',3,(#15246,#15247,#15248,#15249,#15250,
#15251,#15252,#15253,#15254,#15255,#15256,#15257,#15258,#15259,#15260,#15261,
#15262,#15263,#15264,#15265,#15266,#15267),.UNSPECIFIED.,.F.,.F.,(4,3,3,
3,3,3,3,4),(158.202374485951,158.68872269872,159.686764979844,160.684807260968,
161.682849542092,162.680891823216,163.67893410434,164.48555979313),
 .UNSPECIFIED.);
#444=B_SPLINE_CURVE_WITH_KNOTS('',3,(#15272,#15273,#15274,#15275,#15276,
#15277,#15278,#15279,#15280,#15281,#15282,#15283,#15284,#15285,#15286,#15287,
#15288,#15289,#15290,#15291,#15292,#15293,#15294,#15295,#15296),
 .UNSPECIFIED.,.F.,.F.,(4,3,3,3,3,3,3,3,4),(-173.738026814297,-173.589857789537,
-172.592214928677,-171.594572067818,-170.596929206958,-169.599286346099,
-168.60164348524,-167.60400062438,-167.454841507118),.UNSPECIFIED.);
#445=B_SPLINE_CURVE_WITH_KNOTS('',3,(#15297,#15298,#15299,#15300,#15301,
#15302,#15303,#15304,#15305,#15306,#15307,#15308,#15309,#15310,#15311,#15312,
#15313,#15314,#15315,#15316,#15317,#15318,#15319,#15320,#15321),
 .UNSPECIFIED.,.F.,.F.,(4,3,3,3,3,3,3,3,4),(164.48555979313,164.676976385465,
165.675018666588,166.673060947713,167.671103228837,168.669145509961,169.667187791085,
170.665230072209,170.76874510031),.UNSPECIFIED.);
#446=B_SPLINE_CURVE_WITH_KNOTS('',3,(#15326,#15327,#15328,#15329,#15330,
#15331,#15332,#15333,#15334,#15335,#15336,#15337,#15338,#15339,#15340,#15341,
#15342,#15343,#15344,#15345,#15346,#15347),.UNSPECIFIED.,.F.,.F.,(4,3,3,
3,3,3,3,4),(-180.021212121477,-179.575714954693,-178.578072093834,-177.580429232974,
-176.582786372115,-175.585143511255,-174.587500650396,-173.738026814297),
 .UNSPECIFIED.);
#447=B_SPLINE_CURVE_WITH_KNOTS('',3,(#15348,#15349,#15350,#15351,#15352,
#15353,#15354,#15355,#15356,#15357,#15358,#15359,#15360,#15361,#15362,#15363,
#15364,#15365,#15366,#15367,#15368,#15369),.UNSPECIFIED.,.F.,.F.,(4,3,3,
3,3,3,3,4),(170.76874510031,171.663272353333,172.661314634457,173.659356915581,
174.657399196705,175.655441477829,176.653483758953,177.051930407489),
 .UNSPECIFIED.);
#448=B_SPLINE_CURVE_WITH_KNOTS('',3,(#15374,#15375,#15376,#15377,#15378,
#15379,#15380,#15381,#15382,#15383,#15384,#15385,#15386,#15387,#15388,#15389,
#15390,#15391,#15392,#15393,#15394,#15395),.UNSPECIFIED.,.F.,.F.,(4,3,3,
3,3,3,3,4),(-186.304397428656,-185.56157211985,-184.56392925899,-183.566286398131,
-182.568643537271,-181.571000676412,-180.573357815553,-180.021212121477),
 .UNSPECIFIED.);
#449=B_SPLINE_CURVE_WITH_KNOTS('',3,(#15396,#15397,#15398,#15399,#15400,
#15401,#15402,#15403,#15404,#15405,#15406,#15407,#15408,#15409,#15410,#15411,
#15412,#15413,#15414,#15415,#15416,#15417),.UNSPECIFIED.,.F.,.F.,(4,3,3,
3,3,3,3,4),(177.051930407489,177.651526040077,178.649568321201,179.647610602325,
180.645652883449,181.643695164573,182.641737445697,183.335115714669),
 .UNSPECIFIED.);
#450=B_SPLINE_CURVE_WITH_KNOTS('',3,(#15423,#15424,#15425,#15426,#15427,
#15428,#15429,#15430,#15431,#15432),.UNSPECIFIED.,.F.,.F.,(4,1,1,1,1,1,
1,4),(197.920337176157,198.17515472821,199.172797589069,200.170440449928,
201.168083310788,202.165726171647,203.163369032507,204.161011893366),
 .UNSPECIFIED.);
#451=B_SPLINE_CURVE_WITH_KNOTS('',3,(#15435,#15436,#15437,#15438,#15439,
#15440,#15441,#15442,#15443),.UNSPECIFIED.,.F.,.F.,(4,1,1,1,1,1,4),(197.920337176157,
197.930069567874,198.928111848998,199.926154130122,200.924196411246,201.92223869237,
202.920280973494),.UNSPECIFIED.);
#452=B_SPLINE_CURVE_WITH_KNOTS('',3,(#15448,#15449,#15450,#15451,#15452,
#15453,#15454,#15455,#15456,#15457),.UNSPECIFIED.,.F.,.F.,(4,1,1,1,1,1,
1,4),(191.637151868977,192.189297563053,193.186940423913,194.184583284772,
195.182226145631,196.179869006491,197.17751186735,197.920337176157),
 .UNSPECIFIED.);
#453=B_SPLINE_CURVE_WITH_KNOTS('',3,(#15458,#15459,#15460,#15461,#15462,
#15463,#15464,#15465,#15466,#15467),.UNSPECIFIED.,.F.,.F.,(4,1,1,1,1,1,
1,4),(191.637151868977,191.94181588113,192.939858162254,193.937900443378,
194.935942724502,195.933985005626,196.93202728675,197.920337176157),
 .UNSPECIFIED.);
#454=B_SPLINE_CURVE_WITH_KNOTS('',3,(#15472,#15473,#15474,#15475,#15476,
#15477,#15478,#15479,#15480,#15481),.UNSPECIFIED.,.F.,.F.,(4,1,1,1,1,1,
1,4),(185.353966561798,186.203440397897,187.201083258756,188.198726119616,
189.196368980475,190.194011841334,191.191654702194,191.637151868977),
 .UNSPECIFIED.);
#455=B_SPLINE_CURVE_WITH_KNOTS('',3,(#15482,#15483,#15484,#15485,#15486,
#15487,#15488,#15489,#15490,#15491),.UNSPECIFIED.,.F.,.F.,(4,1,1,1,1,1,
1,4),(185.353966561798,185.953562194385,186.951604475509,187.949646756633,
188.947689037757,189.945731318881,190.943773600006,191.637151868977),
 .UNSPECIFIED.);
#456=B_SPLINE_CURVE_WITH_KNOTS('',3,(#15496,#15497,#15498,#15499,#15500,
#15501,#15502,#15503,#15504,#15505,#15506),.UNSPECIFIED.,.F.,.F.,(4,1,1,
1,1,1,1,1,4),(179.070781254618,179.219940371881,180.21758323274,181.2152260936,
182.212868954459,183.210511815318,184.208154676178,185.205797537037,185.353966561798),
 .UNSPECIFIED.);
#457=B_SPLINE_CURVE_WITH_KNOTS('',3,(#15507,#15508,#15509,#15510,#15511,
#15512,#15513,#15514,#15515,#15516),.UNSPECIFIED.,.F.,.F.,(4,1,1,1,1,1,
1,4),(179.070781254618,179.965308507641,180.963350788765,181.961393069889,
182.959435351013,183.957477632137,184.955519913261,185.353966561798),
 .UNSPECIFIED.);
#458=B_SPLINE_CURVE_WITH_KNOTS('',3,(#15521,#15522,#15523,#15524,#15525,
#15526,#15527,#15528,#15529,#15530),.UNSPECIFIED.,.F.,.F.,(4,1,1,1,1,1,
1,4),(172.787595947439,173.234083206724,174.231726067584,175.229368928443,
176.227011789303,177.224654650162,178.222297511021,179.070781254618),
 .UNSPECIFIED.);
#459=B_SPLINE_CURVE_WITH_KNOTS('',3,(#15531,#15532,#15533,#15534,#15535,
#15536,#15537,#15538,#15539,#15540,#15541),.UNSPECIFIED.,.F.,.F.,(4,1,1,
1,1,1,1,1,4),(172.787595947439,172.979012539773,173.977054820897,174.975097102021,
175.973139383145,176.971181664269,177.969223945393,178.967266226517,179.070781254618),
 .UNSPECIFIED.);
#460=B_SPLINE_CURVE_WITH_KNOTS('',3,(#15546,#15547,#15548,#15549,#15550,
#15551,#15552,#15553,#15554,#15555),.UNSPECIFIED.,.F.,.F.,(4,1,1,1,1,1,
1,4),(166.504410640259,167.248226041568,168.245868902427,169.243511763287,
170.241154624146,171.238797485006,172.236440345865,172.787595947439),
 .UNSPECIFIED.);
#461=B_SPLINE_CURVE_WITH_KNOTS('',3,(#15556,#15557,#15558,#15559,#15560,
#15561,#15562,#15563,#15564,#15565),.UNSPECIFIED.,.F.,.F.,(4,1,1,1,1,1,
1,4),(166.504410640259,166.990758853029,167.988801134153,168.986843415277,
169.984885696401,170.982927977525,171.980970258649,172.787595947439),
 .UNSPECIFIED.);
#462=B_SPLINE_CURVE_WITH_KNOTS('',3,(#15570,#15571,#15572,#15573,#15574,
#15575,#15576,#15577,#15578,#15579,#15580),.UNSPECIFIED.,.F.,.F.,(4,1,1,
1,1,1,1,1,4),(160.22122533308,160.264726015552,161.262368876412,162.260011737271,
163.25765459813,164.25529745899,165.252940319849,166.250583180709,166.504410640259),
 .UNSPECIFIED.);
#463=B_SPLINE_CURVE_WITH_KNOTS('',3,(#15581,#15582,#15583,#15584,#15585,
#15586,#15587,#15588,#15589,#15590),.UNSPECIFIED.,.F.,.F.,(4,1,1,1,1,1,
1,4),(160.22122533308,161.002505166285,162.000547447409,162.998589728533,
163.996632009657,164.994674290781,165.992716571905,166.504410640259),
 .UNSPECIFIED.);
#464=B_SPLINE_CURVE_WITH_KNOTS('',3,(#15595,#15596,#15597,#15598,#15599,
#15600,#15601,#15602,#15603,#15604),.UNSPECIFIED.,.F.,.F.,(4,1,1,1,1,1,
1,4),(153.9380400259,154.278868850396,155.276511711255,156.274154572115,
157.271797432974,158.269440293833,159.267083154693,160.22122533308),
 .UNSPECIFIED.);
#465=B_SPLINE_CURVE_WITH_KNOTS('',3,(#15605,#15606,#15607,#15608,#15609,
#15610,#15611,#15612,#15613,#15614,#15615),.UNSPECIFIED.,.F.,.F.,(4,1,1,
1,1,1,1,1,4),(153.9380400259,154.016209198417,155.014251479541,156.012293760665,
157.010336041789,158.008378322913,159.006420604037,160.004462885161,160.22122533308),
 .UNSPECIFIED.);
#466=B_SPLINE_CURVE_WITH_KNOTS('',3,(#15620,#15621,#15622,#15623,#15624,
#15625,#15626,#15627,#15628,#15629),.UNSPECIFIED.,.F.,.F.,(4,1,1,1,1,1,
1,4),(147.65485471872,148.293011685239,149.290654546099,150.288297406958,
151.285940267817,152.283583128677,153.281225989536,153.9380400259),
 .UNSPECIFIED.);
#467=B_SPLINE_CURVE_WITH_KNOTS('',3,(#15630,#15631,#15632,#15633,#15634,
#15635,#15636,#15637,#15638,#15639),.UNSPECIFIED.,.F.,.F.,(4,1,1,1,1,1,
1,4),(147.65485471872,148.027955511672,149.025997792796,150.02404007392,
151.022082355044,152.020124636168,153.018166917292,153.9380400259),
 .UNSPECIFIED.);
#468=B_SPLINE_CURVE_WITH_KNOTS('',3,(#15644,#15645,#15646,#15647,#15648,
#15649,#15650,#15651,#15652,#15653),.UNSPECIFIED.,.F.,.F.,(4,1,1,1,1,1,
1,4),(141.371669411541,142.307154520083,143.304797380942,144.302440241802,
145.300083102661,146.29772596352,147.29536882438,147.65485471872),
 .UNSPECIFIED.);
#469=B_SPLINE_CURVE_WITH_KNOTS('',3,(#15654,#15655,#15656,#15657,#15658,
#15659,#15660,#15661,#15662,#15663),.UNSPECIFIED.,.F.,.F.,(4,1,1,1,1,1,
1,4),(141.371669411541,142.039701824928,143.037744106052,144.035786387176,
145.0338286683,146.031870949424,147.029913230548,147.65485471872),
 .UNSPECIFIED.);
#470=B_SPLINE_CURVE_WITH_KNOTS('',3,(#15668,#15669,#15670,#15671,#15672,
#15673,#15674,#15675,#15676,#15677,#15678),.UNSPECIFIED.,.F.,.F.,(4,1,1,
1,1,1,1,1,4),(135.088484104361,135.323654494067,136.321297354926,137.318940215786,
138.316583076645,139.314225937505,140.311868798364,141.309511659223,141.371669411541),
 .UNSPECIFIED.);
#471=B_SPLINE_CURVE_WITH_KNOTS('',3,(#15679,#15680,#15681,#15682,#15683,
#15684,#15685,#15686,#15687,#15688),.UNSPECIFIED.,.F.,.F.,(4,1,1,1,1,1,
1,4),(135.088484104361,136.051448138184,137.049490419308,138.047532700432,
139.045574981556,140.04361726268,141.041659543804,141.371669411541),
 .UNSPECIFIED.);
#472=B_SPLINE_CURVE_WITH_KNOTS('',3,(#15693,#15694,#15695,#15696,#15697,
#15698,#15699,#15700,#15701,#15702),.UNSPECIFIED.,.F.,.F.,(4,1,1,1,1,1,
1,4),(128.805298797182,129.337797328911,130.33544018977,131.333083050629,
132.330725911489,133.328368772348,134.326011633208,135.088484104361),
 .UNSPECIFIED.);
#473=B_SPLINE_CURVE_WITH_KNOTS('',3,(#15703,#15704,#15705,#15706,#15707,
#15708,#15709,#15710,#15711,#15712,#15713),.UNSPECIFIED.,.F.,.F.,(4,1,1,
1,1,1,1,1,4),(128.805298797182,129.065152170316,130.06319445144,131.061236732564,
132.059279013688,133.057321294812,134.055363575936,135.05340585706,135.088484104361),
 .UNSPECIFIED.);
#474=B_SPLINE_CURVE_WITH_KNOTS('',3,(#15718,#15719,#15720,#15721,#15722,
#15723,#15724,#15725,#15726,#15727),.UNSPECIFIED.,.F.,.F.,(4,1,1,1,1,1,
1,4),(122.522113490002,123.351940163754,124.349583024614,125.347225885473,
126.344868746332,127.342511607192,128.340154468051,128.805298797182),
 .UNSPECIFIED.);
#475=B_SPLINE_CURVE_WITH_KNOTS('',3,(#15728,#15729,#15730,#15731,#15732,
#15733,#15734,#15735,#15736,#15737),.UNSPECIFIED.,.F.,.F.,(4,1,1,1,1,1,
1,4),(122.522113490002,123.076898483572,124.074940764696,125.07298304582,
126.071025326944,127.069067608068,128.067109889192,128.805298797182),
 .UNSPECIFIED.);
#476=B_SPLINE_CURVE_WITH_KNOTS('',3,(#15742,#15743,#15744,#15745,#15746,
#15747,#15748,#15749,#15750,#15751,#15752),.UNSPECIFIED.,.F.,.F.,(4,1,1,
1,1,1,1,1,4),(116.238928182823,116.368440137738,117.366082998598,118.363725859457,
119.361368720316,120.359011581176,121.356654442035,122.354297302895,122.522113490002),
 .UNSPECIFIED.);
#477=B_SPLINE_CURVE_WITH_KNOTS('',3,(#15753,#15754,#15755,#15756,#15757,
#15758,#15759,#15760,#15761,#15762),.UNSPECIFIED.,.F.,.F.,(4,1,1,1,1,1,
1,4),(116.238928182823,117.088644796828,118.086687077952,119.084729359076,
120.0827716402,121.080813921324,122.078856202448,122.522113490002),
 .UNSPECIFIED.);
#478=B_SPLINE_CURVE_WITH_KNOTS('',3,(#15767,#15768,#15769,#15770,#15771,
#15772,#15773,#15774,#15775,#15776),.UNSPECIFIED.,.F.,.F.,(4,1,1,1,1,1,
1,4),(109.955742875643,110.382582972582,111.380225833441,112.377868694301,
113.37551155516,114.373154416019,115.370797276879,116.238928182823),
 .UNSPECIFIED.);
#479=B_SPLINE_CURVE_WITH_KNOTS('',3,(#15777,#15778,#15779,#15780,#15781,
#15782,#15783,#15784,#15785,#15786,#15787),.UNSPECIFIED.,.F.,.F.,(4,1,1,
1,1,1,1,1,4),(109.955742875643,110.102348828959,111.100391110083,112.098433391207,
113.096475672331,114.094517953455,115.092560234579,116.090602515703,116.238928182823),
 .UNSPECIFIED.);
#480=B_SPLINE_CURVE_WITH_KNOTS('',3,(#15792,#15793,#15794,#15795,#15796,
#15797,#15798,#15799,#15800,#15801),.UNSPECIFIED.,.F.,.F.,(4,1,1,1,1,1,
1,4),(103.672557568463,104.396725807425,105.394368668285,106.392011529144,
107.389654390004,108.387297250863,109.384940111722,109.955742875643),
 .UNSPECIFIED.);
#481=B_SPLINE_CURVE_WITH_KNOTS('',3,(#15802,#15803,#15804,#15805,#15806,
#15807,#15808,#15809,#15810,#15811),.UNSPECIFIED.,.F.,.F.,(4,1,1,1,1,1,
1,4),(103.672557568463,104.114095142215,105.112137423339,106.110179704463,
107.108221985587,108.106264266711,109.104306547835,109.955742875643),
 .UNSPECIFIED.);
#482=B_SPLINE_CURVE_WITH_KNOTS('',3,(#15816,#15817,#15818,#15819,#15820,
#15821,#15822,#15823,#15824,#15825,#15826),.UNSPECIFIED.,.F.,.F.,(4,1,1,
1,1,1,1,1,4),(97.3893722612837,97.4132257814096,98.410868642269,99.4085115031284,
100.406154363988,101.403797224847,102.401440085707,103.399082946566,103.672557568463),
 .UNSPECIFIED.);
#483=B_SPLINE_CURVE_WITH_KNOTS('',3,(#15827,#15828,#15829,#15830,#15831,
#15832,#15833,#15834,#15835,#15836),.UNSPECIFIED.,.F.,.F.,(4,1,1,1,1,1,
1,4),(97.3893722612838,98.125841455471,99.123883736595,100.121926017719,
101.119968298843,102.118010579967,103.116052861091,103.672557568463),
 .UNSPECIFIED.);
#484=B_SPLINE_CURVE_WITH_KNOTS('',3,(#15841,#15842,#15843,#15844,#15845,
#15846,#15847,#15848,#15849,#15850),.UNSPECIFIED.,.F.,.F.,(4,1,1,1,1,1,
1,4),(91.1061869541041,91.4273686162531,92.4250114771125,93.4226543379719,
94.4202971988313,95.4179400596907,96.4155829205502,97.3893722612837),
 .UNSPECIFIED.);
#485=B_SPLINE_CURVE_WITH_KNOTS('',3,(#15851,#15852,#15853,#15854,#15855,
#15856,#15857,#15858,#15859,#15860,#15861),.UNSPECIFIED.,.F.,.F.,(4,1,1,
1,1,1,1,1,4),(91.1061869541042,91.1395454876028,92.1375877687268,93.1356300498508,
94.1336723309749,95.1317146120989,96.1297568932229,97.127799174347,97.3893722612838),
 .UNSPECIFIED.);
#486=B_SPLINE_CURVE_WITH_KNOTS('',3,(#15866,#15867,#15868,#15869,#15870,
#15871,#15872,#15873,#15874,#15875),.UNSPECIFIED.,.F.,.F.,(4,1,1,1,1,1,
1,4),(84.8230016469245,85.4415114510967,86.4391543119561,87.4367971728155,
88.4344400336749,89.4320828945343,90.4297257553937,91.1061869541041),
 .UNSPECIFIED.);
#487=B_SPLINE_CURVE_WITH_KNOTS('',3,(#15876,#15877,#15878,#15879,#15880,
#15881,#15882,#15883,#15884,#15885),.UNSPECIFIED.,.F.,.F.,(4,1,1,1,1,1,
1,4),(84.8230016469246,85.1512918008586,86.1493340819827,87.1473763631067,
88.1454186442307,89.1434609253548,90.1415032064788,91.1061869541042),
 .UNSPECIFIED.);
#488=B_SPLINE_CURVE_WITH_KNOTS('',3,(#15890,#15891,#15892,#15893,#15894,
#15895,#15896,#15897,#15898,#15899),.UNSPECIFIED.,.F.,.F.,(4,1,1,1,1,1,
1,4),(78.539816339745,79.4556542859402,80.4532971467996,81.4509400076591,
82.4485828685185,83.4462257293779,84.4438685902373,84.8230016469245),
 .UNSPECIFIED.);
#489=B_SPLINE_CURVE_WITH_KNOTS('',3,(#15900,#15901,#15902,#15903,#15904,
#15905,#15906,#15907,#15908,#15909),.UNSPECIFIED.,.F.,.F.,(4,1,1,1,1,1,
1,4),(78.539816339745,79.1630381141145,80.1610803952385,81.1591226763625,
82.1571649574865,83.1552072386106,84.1532495197346,84.8230016469246),
 .UNSPECIFIED.);
#490=B_SPLINE_CURVE_WITH_KNOTS('',3,(#15914,#15915,#15916,#15917,#15918,
#15919,#15920,#15921,#15922,#15923,#15924),.UNSPECIFIED.,.F.,.F.,(4,1,1,
1,1,1,1,1,4),(72.2566310325654,72.4721542599244,73.4697971207838,74.4674399816432,
75.4650828425026,76.462725703362,77.4603685642214,78.4580114250808,78.539816339745),
 .UNSPECIFIED.);
#491=B_SPLINE_CURVE_WITH_KNOTS('',3,(#15925,#15926,#15927,#15928,#15929,
#15930,#15931,#15932,#15933,#15934),.UNSPECIFIED.,.F.,.F.,(4,1,1,1,1,1,
1,4),(72.2566310325654,73.1747844273703,74.1728267084943,75.1708689896184,
76.1689112707424,77.1669535518664,78.1649958329905,78.539816339745),
 .UNSPECIFIED.);
#492=B_SPLINE_CURVE_WITH_KNOTS('',3,(#15939,#15940,#15941,#15942,#15943,
#15944,#15945,#15946,#15947,#15948),.UNSPECIFIED.,.F.,.F.,(4,1,1,1,1,1,
1,4),(65.9734457253858,66.486297094768,67.4839399556274,68.4815828164868,
69.4792256773462,70.4768685382056,71.474511399065,72.2566310325654),
 .UNSPECIFIED.);
#493=B_SPLINE_CURVE_WITH_KNOTS('',3,(#15949,#15950,#15951,#15952,#15953,
#15954,#15955,#15956,#15957,#15958,#15959),.UNSPECIFIED.,.F.,.F.,(4,1,1,
1,1,1,1,1,4),(65.9734457253858,66.1884884595021,67.1865307406262,68.1845730217502,
69.1826153028742,70.1806575839982,71.1786998651223,72.1767421462463,72.2566310325654),
 .UNSPECIFIED.);
#494=B_SPLINE_CURVE_WITH_KNOTS('',3,(#15964,#15965,#15966,#15967,#15968,
#15969,#15970,#15971,#15972,#15973),.UNSPECIFIED.,.F.,.F.,(4,1,1,1,1,1,
1,4),(59.6902604182062,60.5004399296115,61.4980827904709,62.4957256513303,
63.4933685121897,64.4910113730492,65.4886542339086,65.9734457253858),
 .UNSPECIFIED.);
#495=B_SPLINE_CURVE_WITH_KNOTS('',3,(#15974,#15975,#15976,#15977,#15978,
#15979,#15980,#15981,#15982,#15983),.UNSPECIFIED.,.F.,.F.,(4,1,1,1,1,1,
1,4),(59.6902604182062,60.200234772758,61.198277053882,62.196319335006,
63.19436161613,64.1924038972541,65.1904461783781,65.9734457253858),
 .UNSPECIFIED.);
#496=B_SPLINE_CURVE_WITH_KNOTS('',3,(#15988,#15989,#15990,#15991,#15992,
#15993,#15994,#15995,#15996,#15997,#15998),.UNSPECIFIED.,.F.,.F.,(4,1,1,
1,1,1,1,1,4),(53.4070751110266,53.5169399035957,54.5145827644551,55.5122256253145,
56.5098684861739,57.5075113470333,58.5051542078927,59.5027970687521,59.6902604182062),
 .UNSPECIFIED.);
#497=B_SPLINE_CURVE_WITH_KNOTS('',3,(#15999,#16000,#16001,#16002,#16003,
#16004,#16005,#16006,#16007,#16008),.UNSPECIFIED.,.F.,.F.,(4,1,1,1,1,1,
1,4),(53.4070751110266,54.2119810860138,55.2100233671378,56.2080656482619,
57.2061079293859,58.2041502105099,59.2021924916339,59.6902604182062),
 .UNSPECIFIED.);
#498=B_SPLINE_CURVE_WITH_KNOTS('',3,(#16013,#16014,#16015,#16016,#16017,
#16018,#16019,#16020,#16021,#16022),.UNSPECIFIED.,.F.,.F.,(4,1,1,1,1,1,
1,4),(47.123889803847,47.5310827384393,48.5287255992987,49.5263684601581,
50.5240113210175,51.5216541818769,52.5192970427363,53.4070751110266),
 .UNSPECIFIED.);
#499=B_SPLINE_CURVE_WITH_KNOTS('',3,(#16023,#16024,#16025,#16026,#16027,
#16028,#16029,#16030,#16031,#16032,#16033),.UNSPECIFIED.,.F.,.F.,(4,1,1,
1,1,1,1,1,4),(47.123889803847,47.2256851181456,48.2237273992696,49.2217696803937,
50.2198119615177,51.2178542426417,52.2158965237657,53.2139388048898,53.4070751110266),
 .UNSPECIFIED.);
#500=B_SPLINE_CURVE_WITH_KNOTS('',3,(#16038,#16039,#16040,#16041,#16042,
#16043,#16044,#16045,#16046,#16047),.UNSPECIFIED.,.F.,.F.,(4,1,1,1,1,1,
1,4),(40.8407044966674,41.5452255732828,42.5428684341422,43.5405112950016,
44.538154155861,45.5357970167204,46.5334398775799,47.123889803847),
 .UNSPECIFIED.);
#501=B_SPLINE_CURVE_WITH_KNOTS('',3,(#16048,#16049,#16050,#16051,#16052,
#16053,#16054,#16055,#16056,#16057),.UNSPECIFIED.,.F.,.F.,(4,1,1,1,1,1,
1,4),(40.8407044966675,41.2374314314014,42.2354737125255,43.2335159936495,
44.2315582747735,45.2296005558975,46.2276428370216,47.123889803847),
 .UNSPECIFIED.);
#502=B_SPLINE_CURVE_WITH_KNOTS('',3,(#16062,#16063,#16064,#16065,#16066,
#16067,#16068,#16069,#16070,#16071,#16072),.UNSPECIFIED.,.F.,.F.,(4,1,1,
1,1,1,1,1,4),(34.5575191894878,34.561725547267,35.5593684081264,36.5570112689858,
37.5546541298452,38.5522969907046,39.549939851564,40.5475827124234,40.8407044966674),
 .UNSPECIFIED.);
#503=B_SPLINE_CURVE_WITH_KNOTS('',3,(#16073,#16074,#16075,#16076,#16077,
#16078,#16079,#16080,#16081,#16082),.UNSPECIFIED.,.F.,.F.,(4,1,1,1,1,1,
1,4),(34.5575191894879,35.2491777446573,36.2472200257813,37.2452623069053,
38.2433045880294,39.2413468691534,40.2393891502774,40.8407044966675),
 .UNSPECIFIED.);
#504=B_SPLINE_CURVE_WITH_KNOTS('',3,(#16087,#16088,#16089,#16090,#16091,
#16092,#16093,#16094,#16095,#16096),.UNSPECIFIED.,.F.,.F.,(4,1,1,1,1,1,
1,4),(28.2743338823082,28.5758683821105,29.5735112429699,30.5711541038294,
31.5687969646888,32.5664398255482,33.5640826864076,34.5575191894878),
 .UNSPECIFIED.);
#505=B_SPLINE_CURVE_WITH_KNOTS('',3,(#16097,#16098,#16099,#16100,#16101,
#16102,#16103,#16104,#16105,#16106),.UNSPECIFIED.,.F.,.F.,(4,1,1,1,1,1,
1,4),(28.2743338823083,29.2609240579131,30.2589663390371,31.2570086201612,
32.2550509012852,33.2530931824092,34.2511354635333,34.5575191894879),
 .UNSPECIFIED.);
#506=B_SPLINE_CURVE_WITH_KNOTS('',3,(#16111,#16112,#16113,#16114,#16115,
#16116,#16117,#16118,#16119,#16120),.UNSPECIFIED.,.F.,.F.,(4,1,1,1,1,1,
1,4),(21.9911485751286,22.5900112169541,23.5876540778135,24.5852969386729,
25.5829397995323,26.5805826603917,27.5782255212511,28.2743338823082),
 .UNSPECIFIED.);
#507=B_SPLINE_CURVE_WITH_KNOTS('',3,(#16121,#16122,#16123,#16124,#16125,
#16126,#16127,#16128,#16129,#16130,#16131),.UNSPECIFIED.,.F.,.F.,(4,1,1,
1,1,1,1,1,4),(21.9911485751287,22.2746280900449,23.272670371169,24.270712652293,
25.268754933417,26.266797214541,27.2648394956651,28.2628817767891,28.2743338823083),
 .UNSPECIFIED.);
#508=B_SPLINE_CURVE_WITH_KNOTS('',3,(#16136,#16137,#16138,#16139,#16140,
#16141,#16142,#16143,#16144,#16145),.UNSPECIFIED.,.F.,.F.,(4,1,1,1,1,1,
1,4),(15.707963267949,16.6041540517977,17.6017969126571,18.5994397735165,
19.5970826343759,20.5947254952353,21.5923683560947,21.9911485751286),
 .UNSPECIFIED.);
#509=B_SPLINE_CURVE_WITH_KNOTS('',3,(#16146,#16147,#16148,#16149,#16150,
#16151,#16152,#16153,#16154,#16155),.UNSPECIFIED.,.F.,.F.,(4,1,1,1,1,1,
1,4),(15.7079632679491,16.2863744033008,17.2844166844248,18.2824589655488,
19.2805012466728,20.2785435277969,21.2765858089209,21.9911485751287),
 .UNSPECIFIED.);
#510=B_SPLINE_CURVE_WITH_KNOTS('',3,(#16158,#16159,#16160,#16161,#16162,
#16163,#16164,#16165,#16166,#16167,#16168,#16169,#16170,#16171,#16172,#16173,
#16174,#16175,#16176,#16177,#16178,#16179,#16180,#16181,#16182,#16183,#16184,
#16185,#16186,#16187,#16188,#16189,#16190,#16191,#16192,#16193,#16194,#16195,
#16196,#16197,#16198,#16199,#16200,#16201,#16202,#16203,#16204,#16205,#16206,
#16207,#16208,#16209,#16210,#16211,#16212,#16213,#16214,#16215,#16216,#16217,
#16218,#16219,#16220,#16221,#16222,#16223,#16224,#16225,#16226,#16227,#16228,
#16229,#16230,#16231,#16232,#16233,#16234,#16235,#16236,#16237,#16238,#16239,
#16240,#16241,#16242,#16243,#16244,#16245,#16246,#16247,#16248,#16249,#16250,
#16251,#16252,#16253,#16254,#16255,#16256,#16257,#16258,#16259,#16260,#16261,
#16262,#16263,#16264,#16265,#16266,#16267,#16268,#16269,#16270,#16271,#16272,
#16273,#16274,#16275,#16276,#16277,#16278),.UNSPECIFIED.,.F.,.F.,(4,3,3,
3,3,3,3,3,3,3,3,3,3,3,3,3,3,3,3,3,3,3,3,3,3,3,3,3,3,3,3,3,3,3,3,3,3,3,3,
3,4),(-0.753008129282056,-0.726412283548368,-0.715911613874471,-0.694893371653716,
-0.683361029549332,-0.673826434412814,-0.652889016486892,-0.639679181765185,
-0.63195159856097,-0.60480408471638,-0.59150990338668,-0.582561183693184,
-0.554067746128576,-0.540494882749548,-0.528208608719221,-0.505843484121927,
-0.4921308028701,-0.483102814228457,-0.456032674248847,-0.436199115577779,
-0.427073928162626,-0.400948091236321,-0.382860905241332,-0.374822254310016,
-0.34584221065474,-0.333939649620793,-0.324058619604945,-0.29393738163796,
-0.278576588250954,-0.269234263278142,-0.238815915606663,-0.225742435796944,
-0.216239773488962,-0.18666367230127,-0.170750005528772,-0.161294486761502,
-0.129614927749849,-0.114924930935507,-0.106250072717365,-0.0979353687381955,
-0.0965360155478562),.UNSPECIFIED.);
#511=B_SPLINE_CURVE_WITH_KNOTS('',3,(#16280,#16281,#16282,#16283,#16284,
#16285,#16286,#16287,#16288,#16289,#16290,#16291,#16292,#16293,#16294,#16295,
#16296,#16297,#16298,#16299,#16300,#16301,#16302,#16303,#16304,#16305,#16306,
#16307,#16308,#16309,#16310,#16311,#16312,#16313,#16314,#16315,#16316),
 .UNSPECIFIED.,.F.,.F.,(4,3,3,3,3,3,3,3,3,3,3,3,4),(-0.204609524178132,
-0.173922074105667,-0.152149392827302,-0.142793959810126,-0.12983323009626,
-0.11308637627832,-0.0998536142809363,-0.090547498816978,-0.0679106241127335,
-0.0514558350659385,-0.042025593252969,-0.0155529233063705,0.),
 .UNSPECIFIED.);
#512=B_SPLINE_CURVE_WITH_KNOTS('',3,(#16319,#16320,#16321,#16322,#16323,
#16324,#16325,#16326,#16327,#16328,#16329,#16330,#16331,#16332,#16333,#16334),
 .UNSPECIFIED.,.F.,.F.,(4,3,3,3,3,4),(-0.0965360155478562,-0.0724020116608921,
-0.0590232605257019,-0.050388474335024,-0.0186937936910934,0.),
 .UNSPECIFIED.);
#513=B_SPLINE_CURVE_WITH_KNOTS('',3,(#17123,#17124,#17125,#17126,#17127,
#17128,#17129,#17130),.UNSPECIFIED.,.F.,.F.,(4,1,1,1,1,4),(11.6159397475006,
12.61358260836,13.6112254692194,14.6088683300789,15.6065111909383,15.707963267949),
 .UNSPECIFIED.);
#514=B_SPLINE_CURVE_WITH_KNOTS('',3,(#17131,#17132,#17133,#17134,#17135,
#17136,#17137,#17138,#17139,#17140,#17141,#17142,#17143,#17144,#17145,#17146,
#17147,#17148,#17149,#17150,#17151,#17152,#17153,#17154,#17155,#17156,#17157,
#17158,#17159,#17160,#17161,#17162,#17163,#17164,#17165,#17166,#17167,#17168,
#17169,#17170,#17171,#17172,#17173,#17174,#17175,#17176,#17177,#17178,#17179),
 .UNSPECIFIED.,.F.,.F.,(4,3,3,3,3,3,3,3,3,3,3,3,3,3,3,3,4),(-0.275362278356892,
-0.263988733943187,-0.242277787653762,-0.228409792083558,-0.208856161945484,
-0.197709057767663,-0.168075464588018,-0.150222803571495,-0.140083955862437,
-0.125365894046572,-0.0997819296507484,-0.0889593225835958,-0.0667194919376969,
-0.0511923416312717,-0.0404361839568205,-0.0141940669149386,0.),
 .UNSPECIFIED.);
#515=B_SPLINE_CURVE_WITH_KNOTS('',3,(#17180,#17181,#17182,#17183,#17184,
#17185,#17186,#17187,#17188,#17189,#17190,#17191,#17192,#17193,#17194,#17195,
#17196,#17197,#17198),.UNSPECIFIED.,.F.,.F.,(4,3,3,3,3,3,4),(-191.027404416132,
-190.549786424147,-189.552143563287,-188.554500702428,-187.556857841568,
-186.559214980709,-186.304397428656),.UNSPECIFIED.);
#516=B_SPLINE_CURVE_WITH_KNOTS('',3,(#17201,#17202,#17203,#17204,#17205,
#17206,#17207,#17208,#17209),.UNSPECIFIED.,.F.,.F.,(4,1,1,1,1,1,4),(10.3752088276283,
11.2961629976806,12.2942052788047,13.2922475599287,14.2902898410527,15.2883321221767,
15.7079632679491),.UNSPECIFIED.);
#517=B_SPLINE_CURVE_WITH_KNOTS('',3,(#18003,#18004,#18005,#18006,#18007,
#18008,#18009,#18010,#18011,#18012,#18013,#18014,#18015,#18016,#18017,#18018,
#18019,#18020,#18021,#18022,#18023,#18024),.UNSPECIFIED.,.F.,.F.,(4,3,3,
3,3,3,3,4),(183.335115714669,183.639779726821,184.637822007945,185.635864289069,
186.633906570193,187.631948851317,188.629991132441,188.954231742812),
 .UNSPECIFIED.);
#518=B_SPLINE_CURVE_WITH_KNOTS('',3,(#18025,#18026,#18027,#18028,#18029,
#18030,#18031,#18032,#18033,#18034,#18035,#18036,#18037,#18038,#18039,#18040,
#18041,#18042,#18043,#18044,#18045,#18046,#18047,#18048,#18049,#18050,#18051,
#18052,#18053,#18054,#18055,#18056,#18057,#18058,#18059,#18060,#18061,#18062,
#18063,#18064,#18065,#18066,#18067,#18068,#18069,#18070,#18071,#18072,#18073,
#18074,#18075,#18076),.UNSPECIFIED.,.F.,.F.,(4,3,3,3,3,3,3,3,3,3,3,3,3,
3,3,3,3,4),(-0.276631791712714,-0.267404104599176,-0.245529112929484,-0.233826742508505,
-0.212230201958684,-0.201819484750363,-0.173281546649687,-0.162756755581661,
-0.152537502224722,-0.140478169692516,-0.120739781640826,-0.110641775261762,
-0.100726383882944,-0.0755447879122082,-0.0587891884452614,-0.0493012364577666,
-0.0182848522583483,0.),.UNSPECIFIED.);
#519=B_SPLINE_CURVE_WITH_KNOTS('',3,(#18131,#18132,#18133,#18134,#18135,
#18136,#18137),.UNSPECIFIED.,.F.,.F.,(4,3,4),(-30.159289474462,-29.2544199692899,
-28.9853432330879),.UNSPECIFIED.);
#520=B_SPLINE_CURVE_WITH_KNOTS('',3,(#18143,#18144,#18145,#18146,#18147,
#18148,#18149,#18150,#18151,#18152,#18153,#18154,#18155,#18156,#18157,#18158,
#18159,#18160,#18161),.UNSPECIFIED.,.F.,.F.,(4,3,3,3,3,3,4),(26.4423043696954,
27.3041253046706,28.2792726369803,29.25441996929,30.2295673015996,31.2047146339093,
32.179861966219),.UNSPECIFIED.);
#521=B_SPLINE_CURVE_WITH_KNOTS('',3,(#18163,#18164,#18165,#18166,#18167,
#18168,#18169,#18170,#18171,#18172,#18173,#18174,#18175,#18176,#18177,#18178,
#18179,#18180,#18181,#18182,#18183,#18184),.UNSPECIFIED.,.F.,.F.,(4,3,3,
3,3,3,3,4),(-28.9853432330879,-28.2792726369803,-27.3041253046706,-26.3289779723609,
-25.3538306400513,-24.3786833077416,-23.403535975432,-22.7021579259084),
 .UNSPECIFIED.);
#522=B_SPLINE_CURVE_WITH_KNOTS('',3,(#18189,#18190,#18191,#18192,#18193,
#18194,#18195,#18196,#18197,#18198,#18199,#18200,#18201,#18202,#18203,#18204,
#18205,#18206,#18207,#18208,#18209,#18210,#18211,#18212,#18213),
 .UNSPECIFIED.,.F.,.F.,(4,3,3,3,3,3,3,3,4),(20.1591190625159,20.478093978503,
21.4532413108126,22.4283886431223,23.403535975432,24.3786833077416,25.3538306400513,
26.328977972361,26.4423043696954),.UNSPECIFIED.);
#523=B_SPLINE_CURVE_WITH_KNOTS('',3,(#18214,#18215,#18216,#18217,#18218,
#18219,#18220,#18221,#18222,#18223,#18224,#18225,#18226,#18227,#18228,#18229,
#18230,#18231,#18232,#18233,#18234,#18235,#18236,#18237,#18238),
 .UNSPECIFIED.,.F.,.F.,(4,3,3,3,3,3,3,3,4),(-22.7021579259084,-22.4283886431223,
-21.4532413108126,-20.478093978503,-19.5029466461933,-18.5277993138836,
-17.552651981574,-16.5775046492643,-16.4189726187288),.UNSPECIFIED.);
#524=B_SPLINE_CURVE_WITH_KNOTS('',3,(#18243,#18244,#18245,#18246,#18247,
#18248,#18249,#18250,#18251,#18252,#18253,#18254,#18255,#18256,#18257,#18258,
#18259,#18260,#18261,#18262,#18263,#18264),.UNSPECIFIED.,.F.,.F.,(4,3,3,
3,3,3,3,4),(13.8759337553363,14.627209984645,15.6023573169546,16.5775046492643,
17.552651981574,18.5277993138836,19.5029466461933,20.1591190625159),
 .UNSPECIFIED.);
#525=B_SPLINE_CURVE_WITH_KNOTS('',3,(#18265,#18266,#18267,#18268,#18269,
#18270,#18271,#18272,#18273,#18274,#18275,#18276,#18277,#18278,#18279,#18280,
#18281,#18282,#18283,#18284,#18285,#18286),.UNSPECIFIED.,.F.,.F.,(4,3,3,
3,3,3,3,4),(-16.4189726187288,-15.6023573169546,-14.627209984645,-13.6520626523353,
-12.6769153200256,-11.701767987716,-10.7266206554063,-10.1357873115492),
 .UNSPECIFIED.);
#526=B_SPLINE_CURVE_WITH_KNOTS('',3,(#18292,#18293,#18294,#18295,#18296,
#18297,#18298,#18299,#18300,#18301,#18302,#18303,#18304),.UNSPECIFIED.,
 .F.,.F.,(4,3,3,3,4),(-3.8526020043696,-2.92544199692899,-1.95029466461933,
-0.975147332309664,0.),.UNSPECIFIED.);
#527=B_SPLINE_CURVE_WITH_KNOTS('',3,(#18307,#18308,#18309,#18310,#18311,
#18312,#18313,#18314,#18315,#18316,#18317,#18318,#18319,#18320,#18321,#18322,
#18323,#18324,#18325),.UNSPECIFIED.,.F.,.F.,(4,3,3,3,3,3,4),(2.02057249175693,
2.925441996929,3.90058932923866,4.87573666154832,5.85088399385799,6.82603132616766,
7.59274844815668),.UNSPECIFIED.);
#528=B_SPLINE_CURVE_WITH_KNOTS('',3,(#18331,#18332,#18333,#18334,#18335,
#18336,#18337),.UNSPECIFIED.,.F.,.F.,(4,1,1,1,4),(40.8407044966673,41.1097812328693,
42.084928565179,43.0600758974886,44.0352232297983),.UNSPECIFIED.);
#529=B_SPLINE_CURVE_WITH_KNOTS('',3,(#18340,#18341,#18342,#18343,#18344,
#18345,#18346),.UNSPECIFIED.,.F.,.F.,(4,1,1,1,4),(40.8407044966673,41.7025254316425,
42.6776727639522,43.6528200962618,44.5576896014339),.UNSPECIFIED.);
#530=B_SPLINE_CURVE_WITH_KNOTS('',3,(#18351,#18352,#18353,#18354,#18355,
#18356,#18357,#18358,#18359,#18360),.UNSPECIFIED.,.F.,.F.,(4,1,1,1,1,1,
1,4),(34.5575191894877,35.2588972390113,36.234044571321,37.2091919036307,
38.1843392359403,39.15948656825,40.1346339005596,40.8407044966673),
 .UNSPECIFIED.);
#531=B_SPLINE_CURVE_WITH_KNOTS('',3,(#18361,#18362,#18363,#18364,#18365,
#18366,#18367,#18368,#18369,#18370,#18371),.UNSPECIFIED.,.F.,.F.,(4,1,1,
1,1,1,1,1,4),(34.5575191894877,34.8764941054748,35.8516414377845,36.8267887700942,
37.8019361024038,38.7770834347135,39.7522307670232,40.7273780993328,40.8407044966673),
 .UNSPECIFIED.);
#532=B_SPLINE_CURVE_WITH_KNOTS('',3,(#18376,#18377,#18378,#18379,#18380,
#18381,#18382,#18383,#18384,#18385,#18386),.UNSPECIFIED.,.F.,.F.,(4,1,1,
1,1,1,1,1,4),(28.2743338823081,28.4328659128437,29.4080132451533,30.383160577463,
31.3583079097727,32.3334552420823,33.308602574392,34.2837499067017,34.5575191894877),
 .UNSPECIFIED.);
#533=B_SPLINE_CURVE_WITH_KNOTS('',3,(#18387,#18388,#18389,#18390,#18391,
#18392,#18393,#18394,#18395,#18396),.UNSPECIFIED.,.F.,.F.,(4,1,1,1,1,1,
1,4),(28.2743338823081,29.0256101116168,30.0007574439265,30.9759047762362,
31.9510521085458,32.9261994408555,33.9013467731652,34.5575191894877),
 .UNSPECIFIED.);
#534=B_SPLINE_CURVE_WITH_KNOTS('',3,(#18401,#18402,#18403,#18404,#18405,
#18406,#18407,#18408,#18409,#18410),.UNSPECIFIED.,.F.,.F.,(4,1,1,1,1,1,
1,4),(21.9911485751285,22.5819819189857,23.5571292512954,24.532276583605,
25.5074239159147,26.4825712482243,27.457718580534,28.2743338823081),
 .UNSPECIFIED.);
#535=B_SPLINE_CURVE_WITH_KNOTS('',3,(#18411,#18412,#18413,#18414,#18415,
#18416,#18417,#18418,#18419,#18420,#18421),.UNSPECIFIED.,.F.,.F.,(4,1,1,
1,1,1,1,1,4),(21.9911485751285,22.1995787854492,23.1747261177589,24.1498734500685,
25.1250207823782,26.1001681146879,27.0753154469975,28.0504627793072,28.2743338823081),
 .UNSPECIFIED.);
#536=B_SPLINE_CURVE_WITH_KNOTS('',3,(#18427,#18428,#18429,#18430,#18431),
 .UNSPECIFIED.,.F.,.F.,(4,1,4),(14.3984001269719,15.3735474592815,15.7079632679489),
 .UNSPECIFIED.);
#537=B_SPLINE_CURVE_WITH_KNOTS('',3,(#18434,#18435,#18436,#18437,#18438),
 .UNSPECIFIED.,.F.,.F.,(4,1,4),(13.8759337553363,14.7808032605084,15.7079632679489),
 .UNSPECIFIED.);
#538=B_SPLINE_CURVE_WITH_KNOTS('',3,(#18440,#18441,#18442,#18443,#18444,
#18445,#18446,#18447,#18448,#18449,#18450),.UNSPECIFIED.,.F.,.F.,(4,1,1,
1,1,1,1,1,4),(15.7079632679489,15.755950592818,16.7310979251277,17.7062452574374,
18.681392589747,19.6565399220567,20.6316872543664,21.606834586676,21.9911485751285),
 .UNSPECIFIED.);
#539=B_SPLINE_CURVE_WITH_KNOTS('',3,(#18451,#18452,#18453,#18454,#18455,
#18456,#18457,#18458,#18459,#18460),.UNSPECIFIED.,.F.,.F.,(4,1,1,1,1,1,
1,4),(15.7079632679489,16.3486947915912,17.3238421239009,18.2989894562105,
19.2741367885202,20.2492841208299,21.2244314531395,21.9911485751285),
 .UNSPECIFIED.);
#540=B_SPLINE_CURVE_WITH_KNOTS('',3,(#18605,#18606,#18607,#18608,#18609,
#18610,#18611,#18612,#18613,#18614,#18615,#18616,#18617,#18618,#18619,#18620,
#18621,#18622,#18623,#18624,#18625,#18626,#18627,#18628,#18629,#18630,#18631,
#18632,#18633,#18634,#18635,#18636,#18637,#18638,#18639,#18640,#18641,#18642,
#18643,#18644,#18645,#18646,#18647,#18648,#18649,#18650,#18651,#18652,#18653),
 .UNSPECIFIED.,.F.,.F.,(4,3,3,3,3,3,3,3,3,3,3,3,3,3,3,3,4),(0.,0.0320333804888866,
0.0505515708593653,0.0603413132804416,0.0917900141854983,0.108096115778005,
0.122914675479851,0.145143248337739,0.168151513577436,0.177516949333476,
0.202471322707608,0.21794283081622,0.231200110368267,0.247503117401854,
0.263651632124391,0.277334442830003,0.286347380332244),.UNSPECIFIED.);
#541=B_SPLINE_CURVE_WITH_KNOTS('',3,(#18654,#18655,#18656,#18657,#18658,
#18659,#18660,#18661,#18662,#18663,#18664,#18665,#18666,#18667,#18668,#18669,
#18670,#18671,#18672,#18673,#18674,#18675,#18676,#18677,#18678,#18679,#18680,
#18681,#18682,#18683,#18684,#18685,#18686,#18687,#18688,#18689,#18690,#18691,
#18692,#18693,#18694,#18695,#18696,#18697,#18698,#18699,#18700,#18701,#18702),
 .UNSPECIFIED.,.F.,.F.,(4,3,3,3,3,3,3,3,3,3,3,3,3,3,3,3,4),(0.,0.0274305464075637,
0.0492901149097146,0.0591933555873536,0.0887250095166089,0.100015570674795,
0.108381796308415,0.130826479038955,0.152531076563578,0.162815893631175,
0.190691958353668,0.212372986031639,0.222945305605857,0.245534254906135,
0.257847836118801,0.274320152521146,0.28514280399515),.UNSPECIFIED.);
#542=B_SPLINE_CURVE_WITH_KNOTS('',3,(#18703,#18704,#18705,#18706,#18707,
#18708,#18709,#18710,#18711,#18712,#18713,#18714,#18715,#18716,#18717,#18718,
#18719,#18720,#18721,#18722,#18723,#18724,#18725,#18726,#18727),
 .UNSPECIFIED.,.F.,.F.,(4,3,3,3,3,3,3,3,4),(-10.1357873115492,-9.75147332309665,
-8.77632599078699,-7.80117865847732,-6.82603132616766,-5.85088399385799,
-4.87573666154833,-3.90058932923866,-3.8526020043696),.UNSPECIFIED.);
#543=B_SPLINE_CURVE_WITH_KNOTS('',3,(#18872,#18873,#18874,#18875,#18876,
#18877,#18878,#18879,#18880,#18881,#18882,#18883,#18884,#18885,#18886,#18887,
#18888,#18889,#18890,#18891,#18892,#18893,#18894,#18895,#18896,#18897,#18898,
#18899,#18900,#18901,#18902,#18903,#18904,#18905,#18906,#18907,#18908,#18909,
#18910,#18911,#18912,#18913,#18914,#18915,#18916,#18917,#18918,#18919,#18920),
 .UNSPECIFIED.,.F.,.F.,(4,3,3,3,3,3,3,3,3,3,3,3,3,3,3,3,4),(0.,0.0274305890506951,
0.0492901290331875,0.0591933603491513,0.0887250177779717,0.100015607166709,
0.108381835831352,0.13082647903896,0.152531071764912,0.162815892251191,
0.190691957318683,0.212372984486691,0.22294529735758,0.245534140364172,
0.257847701250626,0.274320152521159,0.285142803995162),.UNSPECIFIED.);
#544=B_SPLINE_CURVE_WITH_KNOTS('',3,(#18921,#18922,#18923,#18924,#18925,
#18926,#18927,#18928,#18929,#18930,#18931,#18932,#18933,#18934,#18935,#18936,
#18937,#18938,#18939,#18940,#18941,#18942,#18943,#18944,#18945),
 .UNSPECIFIED.,.F.,.F.,(4,3,3,3,3,3,3,3,4),(7.59274844815668,7.80117865847732,
8.77632599078698,9.75147332309665,10.7266206554063,11.701767987716,12.6769153200256,
13.6520626523353,13.8759337553363),.UNSPECIFIED.);
#545=B_SPLINE_CURVE_WITH_KNOTS('',3,(#18946,#18947,#18948,#18949,#18950,
#18951,#18952,#18953,#18954,#18955,#18956,#18957,#18958,#18959,#18960,#18961,
#18962,#18963,#18964,#18965,#18966,#18967,#18968,#18969,#18970,#18971,#18972,
#18973,#18974,#18975,#18976,#18977,#18978,#18979,#18980,#18981,#18982,#18983,
#18984,#18985,#18986,#18987,#18988,#18989,#18990,#18991,#18992,#18993,#18994),
 .UNSPECIFIED.,.F.,.F.,(4,3,3,3,3,3,3,3,3,3,3,3,3,3,3,3,4),(0.,0.0320334058164849,
0.0505515938322513,0.0603413311462071,0.0917900214840119,0.108096111687201,
0.122914678304232,0.145143248337743,0.168151527562726,0.177516955081398,
0.202471327018552,0.217942288122009,0.231200024743484,0.24750284136614,
0.263651600306541,0.277334442830014,0.286347380332252),.UNSPECIFIED.);
#546=SHAPE_REPRESENTATION_RELATIONSHIP('SRR','None',#19136,#556);
#547=SHAPE_REPRESENTATION_RELATIONSHIP('SRR','None',#19137,#557);
#548=SHAPE_REPRESENTATION_RELATIONSHIP('SRR','None',#19138,#558);
#549=SHAPE_REPRESENTATION_RELATIONSHIP('SRR','None',#19139,#559);
#550=SHAPE_REPRESENTATION_RELATIONSHIP('SRR','None',#19141,#560);
#551=SHAPE_REPRESENTATION_RELATIONSHIP('SRR','None',#19142,#561);
#552=SHAPE_REPRESENTATION_RELATIONSHIP('SRR','None',#19143,#562);
#553=SHAPE_REPRESENTATION_RELATIONSHIP('SRR','None',#19144,#563);
#554=SHAPE_REPRESENTATION_RELATIONSHIP('SRR','None',#19145,#564);
#555=SHAPE_REPRESENTATION_RELATIONSHIP('SRR','None',#19146,#565);
#556=ADVANCED_BREP_SHAPE_REPRESENTATION('',(#576),#19079);
#557=ADVANCED_BREP_SHAPE_REPRESENTATION('',(#577),#19080);
#558=ADVANCED_BREP_SHAPE_REPRESENTATION('',(#578),#19081);
#559=ADVANCED_BREP_SHAPE_REPRESENTATION('',(#579),#19082);
#560=ADVANCED_BREP_SHAPE_REPRESENTATION('',(#580),#19084);
#561=ADVANCED_BREP_SHAPE_REPRESENTATION('',(#581),#19085);
#562=ADVANCED_BREP_SHAPE_REPRESENTATION('',(#582),#19086);
#563=ADVANCED_BREP_SHAPE_REPRESENTATION('',(#583),#19087);
#564=ADVANCED_BREP_SHAPE_REPRESENTATION('',(#584),#19088);
#565=ADVANCED_BREP_SHAPE_REPRESENTATION('',(#585),#19089);
#566=STYLED_ITEM('',(#19200),#576);
#567=STYLED_ITEM('',(#19200),#577);
#568=STYLED_ITEM('',(#19201),#578);
#569=STYLED_ITEM('',(#19202),#579);
#570=STYLED_ITEM('',(#19203),#580);
#571=STYLED_ITEM('',(#19203),#581);
#572=STYLED_ITEM('',(#19204),#582);
#573=STYLED_ITEM('',(#19202),#583);
#574=STYLED_ITEM('',(#19205),#584);
#575=STYLED_ITEM('',(#19206),#585);
#576=MANIFOLD_SOLID_BREP('Body1',#6820);
#577=MANIFOLD_SOLID_BREP('Body1',#6821);
#578=MANIFOLD_SOLID_BREP('Body1',#6822);
#579=MANIFOLD_SOLID_BREP('Body1',#6823);
#580=MANIFOLD_SOLID_BREP('Body1',#6824);
#581=MANIFOLD_SOLID_BREP('Body1',#6825);
#582=MANIFOLD_SOLID_BREP('Body1',#6826);
#583=MANIFOLD_SOLID_BREP('Body1',#6827);
#584=MANIFOLD_SOLID_BREP('Body1',#6828);
#585=MANIFOLD_SOLID_BREP('Body1',#6829);
#586=FACE_BOUND('',#1212,.T.);
#587=FACE_BOUND('',#1213,.T.);
#588=FACE_BOUND('',#1214,.T.);
#589=FACE_BOUND('',#1223,.T.);
#590=FACE_BOUND('',#1224,.T.);
#591=FACE_BOUND('',#1225,.T.);
#592=FACE_BOUND('',#1245,.T.);
#593=FACE_BOUND('',#1246,.T.);
#594=FACE_BOUND('',#1247,.T.);
#595=FACE_BOUND('',#1256,.T.);
#596=FACE_BOUND('',#1257,.T.);
#597=FACE_BOUND('',#1258,.T.);
#598=FACE_BOUND('',#1262,.T.);
#599=FACE_BOUND('',#1264,.T.);
#600=FACE_BOUND('',#1267,.T.);
#601=FACE_BOUND('',#1279,.T.);
#602=FACE_BOUND('',#1280,.T.);
#603=FACE_BOUND('',#1281,.T.);
#604=FACE_BOUND('',#1288,.T.);
#605=FACE_BOUND('',#1291,.T.);
#606=FACE_BOUND('',#1302,.T.);
#607=FACE_BOUND('',#1304,.T.);
#608=FACE_BOUND('',#1316,.T.);
#609=FACE_BOUND('',#1325,.T.);
#610=FACE_BOUND('',#1326,.T.);
#611=FACE_BOUND('',#1327,.T.);
#612=FACE_BOUND('',#1376,.T.);
#613=FACE_BOUND('',#1377,.T.);
#614=FACE_BOUND('',#1378,.T.);
#615=FACE_BOUND('',#1379,.T.);
#616=FACE_BOUND('',#1380,.T.);
#617=FACE_BOUND('',#1381,.T.);
#618=FACE_BOUND('',#1385,.T.);
#619=FACE_BOUND('',#1386,.T.);
#620=FACE_BOUND('',#1387,.T.);
#621=FACE_BOUND('',#1399,.T.);
#622=FACE_BOUND('',#1407,.T.);
#623=FACE_BOUND('',#1418,.T.);
#624=FACE_BOUND('',#1420,.T.);
#625=FACE_BOUND('',#1432,.T.);
#626=FACE_BOUND('',#1441,.T.);
#627=FACE_BOUND('',#1442,.T.);
#628=FACE_BOUND('',#1443,.T.);
#629=FACE_BOUND('',#1492,.T.);
#630=FACE_BOUND('',#1493,.T.);
#631=FACE_BOUND('',#1494,.T.);
#632=FACE_BOUND('',#1495,.T.);
#633=FACE_BOUND('',#1496,.T.);
#634=FACE_BOUND('',#1497,.T.);
#635=FACE_BOUND('',#1503,.T.);
#636=FACE_BOUND('',#1507,.T.);
#637=FACE_BOUND('',#1511,.T.);
#638=FACE_BOUND('',#1515,.T.);
#639=FACE_BOUND('',#1535,.T.);
#640=FACE_BOUND('',#1536,.T.);
#641=FACE_BOUND('',#1541,.T.);
#642=FACE_BOUND('',#1542,.T.);
#643=FACE_BOUND('',#1543,.T.);
#644=FACE_BOUND('',#1544,.T.);
#645=FACE_BOUND('',#1545,.T.);
#646=FACE_BOUND('',#1546,.T.);
#647=FACE_BOUND('',#1621,.T.);
#648=FACE_BOUND('',#1624,.T.);
#649=FACE_BOUND('',#1640,.T.);
#650=FACE_BOUND('',#1649,.T.);
#651=FACE_BOUND('',#1653,.T.);
#652=FACE_BOUND('',#1655,.T.);
#653=PLANE('',#6952);
#654=PLANE('',#6953);
#655=PLANE('',#6954);
#656=PLANE('',#6955);
#657=PLANE('',#6956);
#658=PLANE('',#6957);
#659=PLANE('',#6958);
#660=PLANE('',#6959);
#661=PLANE('',#6962);
#662=PLANE('',#6963);
#663=PLANE('',#6964);
#664=PLANE('',#6965);
#665=PLANE('',#6966);
#666=PLANE('',#6967);
#667=PLANE('',#6968);
#668=PLANE('',#6969);
#669=PLANE('',#6973);
#670=PLANE('',#6974);
#671=PLANE('',#6975);
#672=PLANE('',#6976);
#673=PLANE('',#6977);
#674=PLANE('',#6978);
#675=PLANE('',#6990);
#676=PLANE('',#6991);
#677=PLANE('',#6992);
#678=PLANE('',#6993);
#679=PLANE('',#6994);
#680=PLANE('',#6995);
#681=PLANE('',#6996);
#682=PLANE('',#6997);
#683=PLANE('',#7002);
#684=PLANE('',#7003);
#685=PLANE('',#7004);
#686=PLANE('',#7005);
#687=PLANE('',#7006);
#688=PLANE('',#7007);
#689=PLANE('',#7008);
#690=PLANE('',#7015);
#691=PLANE('',#7017);
#692=PLANE('',#7021);
#693=PLANE('',#7026);
#694=PLANE('',#7028);
#695=PLANE('',#7030);
#696=PLANE('',#7031);
#697=PLANE('',#7032);
#698=PLANE('',#7039);
#699=PLANE('',#7042);
#700=PLANE('',#7059);
#701=PLANE('',#7064);
#702=PLANE('',#7070);
#703=PLANE('',#7071);
#704=PLANE('',#7072);
#705=PLANE('',#7073);
#706=PLANE('',#7074);
#707=PLANE('',#7075);
#708=PLANE('',#7076);
#709=PLANE('',#7077);
#710=PLANE('',#7079);
#711=PLANE('',#7081);
#712=PLANE('',#7082);
#713=PLANE('',#7083);
#714=PLANE('',#7084);
#715=PLANE('',#7085);
#716=PLANE('',#7086);
#717=PLANE('',#7087);
#718=PLANE('',#7088);
#719=PLANE('',#7089);
#720=PLANE('',#7090);
#721=PLANE('',#7091);
#722=PLANE('',#7095);
#723=PLANE('',#7097);
#724=PLANE('',#7098);
#725=PLANE('',#7099);
#726=PLANE('',#7100);
#727=PLANE('',#7101);
#728=PLANE('',#7102);
#729=PLANE('',#7104);
#730=PLANE('',#7121);
#731=PLANE('',#7140);
#732=PLANE('',#7141);
#733=PLANE('',#7142);
#734=PLANE('',#7144);
#735=PLANE('',#7158);
#736=PLANE('',#7159);
#737=PLANE('',#7160);
#738=PLANE('',#7161);
#739=PLANE('',#7162);
#740=PLANE('',#7163);
#741=PLANE('',#7164);
#742=PLANE('',#7166);
#743=PLANE('',#7167);
#744=PLANE('',#7168);
#745=PLANE('',#7169);
#746=PLANE('',#7170);
#747=PLANE('',#7171);
#748=PLANE('',#7172);
#749=PLANE('',#7178);
#750=PLANE('',#7179);
#751=PLANE('',#7180);
#752=PLANE('',#7181);
#753=PLANE('',#7182);
#754=PLANE('',#7183);
#755=PLANE('',#7184);
#756=PLANE('',#7185);
#757=PLANE('',#7187);
#758=PLANE('',#7189);
#759=PLANE('',#7190);
#760=PLANE('',#7191);
#761=PLANE('',#7192);
#762=PLANE('',#7193);
#763=PLANE('',#7194);
#764=PLANE('',#7195);
#765=PLANE('',#7196);
#766=PLANE('',#7197);
#767=PLANE('',#7198);
#768=PLANE('',#7199);
#769=PLANE('',#7203);
#770=PLANE('',#7205);
#771=PLANE('',#7206);
#772=PLANE('',#7207);
#773=PLANE('',#7208);
#774=PLANE('',#7209);
#775=PLANE('',#7210);
#776=PLANE('',#7212);
#777=PLANE('',#7229);
#778=PLANE('',#7248);
#779=PLANE('',#7249);
#780=PLANE('',#7250);
#781=PLANE('',#7258);
#782=PLANE('',#7263);
#783=PLANE('',#7264);
#784=PLANE('',#7269);
#785=PLANE('',#7270);
#786=PLANE('',#7275);
#787=PLANE('',#7276);
#788=PLANE('',#7281);
#789=PLANE('',#7300);
#790=PLANE('',#7301);
#791=PLANE('',#7302);
#792=PLANE('',#7303);
#793=PLANE('',#7373);
#794=PLANE('',#7374);
#795=PLANE('',#7375);
#796=PLANE('',#7376);
#797=PLANE('',#7377);
#798=PLANE('',#7378);
#799=PLANE('',#7379);
#800=PLANE('',#7380);
#801=PLANE('',#7384);
#802=PLANE('',#7385);
#803=PLANE('',#7403);
#804=PLANE('',#7405);
#805=PLANE('',#7406);
#806=PLANE('',#7407);
#807=PLANE('',#7408);
#808=PLANE('',#7409);
#809=PLANE('',#7410);
#810=PLANE('',#7411);
#811=PLANE('',#7427);
#812=PLANE('',#7428);
#813=FACE_OUTER_BOUND('',#1201,.T.);
#814=FACE_OUTER_BOUND('',#1202,.T.);
#815=FACE_OUTER_BOUND('',#1203,.T.);
#816=FACE_OUTER_BOUND('',#1204,.T.);
#817=FACE_OUTER_BOUND('',#1205,.T.);
#818=FACE_OUTER_BOUND('',#1206,.T.);
#819=FACE_OUTER_BOUND('',#1207,.T.);
#820=FACE_OUTER_BOUND('',#1208,.T.);
#821=FACE_OUTER_BOUND('',#1209,.T.);
#822=FACE_OUTER_BOUND('',#1210,.T.);
#823=FACE_OUTER_BOUND('',#1211,.T.);
#824=FACE_OUTER_BOUND('',#1215,.T.);
#825=FACE_OUTER_BOUND('',#1216,.T.);
#826=FACE_OUTER_BOUND('',#1217,.T.);
#827=FACE_OUTER_BOUND('',#1218,.T.);
#828=FACE_OUTER_BOUND('',#1219,.T.);
#829=FACE_OUTER_BOUND('',#1220,.T.);
#830=FACE_OUTER_BOUND('',#1221,.T.);
#831=FACE_OUTER_BOUND('',#1222,.T.);
#832=FACE_OUTER_BOUND('',#1226,.T.);
#833=FACE_OUTER_BOUND('',#1227,.T.);
#834=FACE_OUTER_BOUND('',#1228,.T.);
#835=FACE_OUTER_BOUND('',#1229,.T.);
#836=FACE_OUTER_BOUND('',#1230,.T.);
#837=FACE_OUTER_BOUND('',#1231,.T.);
#838=FACE_OUTER_BOUND('',#1232,.T.);
#839=FACE_OUTER_BOUND('',#1233,.T.);
#840=FACE_OUTER_BOUND('',#1234,.T.);
#841=FACE_OUTER_BOUND('',#1235,.T.);
#842=FACE_OUTER_BOUND('',#1236,.T.);
#843=FACE_OUTER_BOUND('',#1237,.T.);
#844=FACE_OUTER_BOUND('',#1238,.T.);
#845=FACE_OUTER_BOUND('',#1239,.T.);
#846=FACE_OUTER_BOUND('',#1240,.T.);
#847=FACE_OUTER_BOUND('',#1241,.T.);
#848=FACE_OUTER_BOUND('',#1242,.T.);
#849=FACE_OUTER_BOUND('',#1243,.T.);
#850=FACE_OUTER_BOUND('',#1244,.T.);
#851=FACE_OUTER_BOUND('',#1248,.T.);
#852=FACE_OUTER_BOUND('',#1249,.T.);
#853=FACE_OUTER_BOUND('',#1250,.T.);
#854=FACE_OUTER_BOUND('',#1251,.T.);
#855=FACE_OUTER_BOUND('',#1252,.T.);
#856=FACE_OUTER_BOUND('',#1253,.T.);
#857=FACE_OUTER_BOUND('',#1254,.T.);
#858=FACE_OUTER_BOUND('',#1255,.T.);
#859=FACE_OUTER_BOUND('',#1259,.T.);
#860=FACE_OUTER_BOUND('',#1260,.T.);
#861=FACE_OUTER_BOUND('',#1261,.T.);
#862=FACE_OUTER_BOUND('',#1263,.T.);
#863=FACE_OUTER_BOUND('',#1265,.T.);
#864=FACE_OUTER_BOUND('',#1266,.T.);
#865=FACE_OUTER_BOUND('',#1268,.T.);
#866=FACE_OUTER_BOUND('',#1269,.T.);
#867=FACE_OUTER_BOUND('',#1270,.T.);
#868=FACE_OUTER_BOUND('',#1271,.T.);
#869=FACE_OUTER_BOUND('',#1272,.T.);
#870=FACE_OUTER_BOUND('',#1273,.T.);
#871=FACE_OUTER_BOUND('',#1274,.T.);
#872=FACE_OUTER_BOUND('',#1275,.T.);
#873=FACE_OUTER_BOUND('',#1276,.T.);
#874=FACE_OUTER_BOUND('',#1277,.T.);
#875=FACE_OUTER_BOUND('',#1278,.T.);
#876=FACE_OUTER_BOUND('',#1282,.T.);
#877=FACE_OUTER_BOUND('',#1283,.T.);
#878=FACE_OUTER_BOUND('',#1284,.T.);
#879=FACE_OUTER_BOUND('',#1285,.T.);
#880=FACE_OUTER_BOUND('',#1286,.T.);
#881=FACE_OUTER_BOUND('',#1287,.T.);
#882=FACE_OUTER_BOUND('',#1289,.T.);
#883=FACE_OUTER_BOUND('',#1290,.T.);
#884=FACE_OUTER_BOUND('',#1292,.T.);
#885=FACE_OUTER_BOUND('',#1293,.T.);
#886=FACE_OUTER_BOUND('',#1294,.T.);
#887=FACE_OUTER_BOUND('',#1295,.T.);
#888=FACE_OUTER_BOUND('',#1296,.T.);
#889=FACE_OUTER_BOUND('',#1297,.T.);
#890=FACE_OUTER_BOUND('',#1298,.T.);
#891=FACE_OUTER_BOUND('',#1299,.T.);
#892=FACE_OUTER_BOUND('',#1300,.T.);
#893=FACE_OUTER_BOUND('',#1301,.T.);
#894=FACE_OUTER_BOUND('',#1303,.T.);
#895=FACE_OUTER_BOUND('',#1305,.T.);
#896=FACE_OUTER_BOUND('',#1306,.T.);
#897=FACE_OUTER_BOUND('',#1307,.T.);
#898=FACE_OUTER_BOUND('',#1308,.T.);
#899=FACE_OUTER_BOUND('',#1309,.T.);
#900=FACE_OUTER_BOUND('',#1310,.T.);
#901=FACE_OUTER_BOUND('',#1311,.T.);
#902=FACE_OUTER_BOUND('',#1312,.T.);
#903=FACE_OUTER_BOUND('',#1313,.T.);
#904=FACE_OUTER_BOUND('',#1314,.T.);
#905=FACE_OUTER_BOUND('',#1315,.T.);
#906=FACE_OUTER_BOUND('',#1317,.T.);
#907=FACE_OUTER_BOUND('',#1318,.T.);
#908=FACE_OUTER_BOUND('',#1319,.T.);
#909=FACE_OUTER_BOUND('',#1320,.T.);
#910=FACE_OUTER_BOUND('',#1321,.T.);
#911=FACE_OUTER_BOUND('',#1322,.T.);
#912=FACE_OUTER_BOUND('',#1323,.T.);
#913=FACE_OUTER_BOUND('',#1324,.T.);
#914=FACE_OUTER_BOUND('',#1328,.T.);
#915=FACE_OUTER_BOUND('',#1329,.T.);
#916=FACE_OUTER_BOUND('',#1330,.T.);
#917=FACE_OUTER_BOUND('',#1331,.T.);
#918=FACE_OUTER_BOUND('',#1332,.T.);
#919=FACE_OUTER_BOUND('',#1333,.T.);
#920=FACE_OUTER_BOUND('',#1334,.T.);
#921=FACE_OUTER_BOUND('',#1335,.T.);
#922=FACE_OUTER_BOUND('',#1336,.T.);
#923=FACE_OUTER_BOUND('',#1337,.T.);
#924=FACE_OUTER_BOUND('',#1338,.T.);
#925=FACE_OUTER_BOUND('',#1339,.T.);
#926=FACE_OUTER_BOUND('',#1340,.T.);
#927=FACE_OUTER_BOUND('',#1341,.T.);
#928=FACE_OUTER_BOUND('',#1342,.T.);
#929=FACE_OUTER_BOUND('',#1343,.T.);
#930=FACE_OUTER_BOUND('',#1344,.T.);
#931=FACE_OUTER_BOUND('',#1345,.T.);
#932=FACE_OUTER_BOUND('',#1346,.T.);
#933=FACE_OUTER_BOUND('',#1347,.T.);
#934=FACE_OUTER_BOUND('',#1348,.T.);
#935=FACE_OUTER_BOUND('',#1349,.T.);
#936=FACE_OUTER_BOUND('',#1350,.T.);
#937=FACE_OUTER_BOUND('',#1351,.T.);
#938=FACE_OUTER_BOUND('',#1352,.T.);
#939=FACE_OUTER_BOUND('',#1353,.T.);
#940=FACE_OUTER_BOUND('',#1354,.T.);
#941=FACE_OUTER_BOUND('',#1355,.T.);
#942=FACE_OUTER_BOUND('',#1356,.T.);
#943=FACE_OUTER_BOUND('',#1357,.T.);
#944=FACE_OUTER_BOUND('',#1358,.T.);
#945=FACE_OUTER_BOUND('',#1359,.T.);
#946=FACE_OUTER_BOUND('',#1360,.T.);
#947=FACE_OUTER_BOUND('',#1361,.T.);
#948=FACE_OUTER_BOUND('',#1362,.T.);
#949=FACE_OUTER_BOUND('',#1363,.T.);
#950=FACE_OUTER_BOUND('',#1364,.T.);
#951=FACE_OUTER_BOUND('',#1365,.T.);
#952=FACE_OUTER_BOUND('',#1366,.T.);
#953=FACE_OUTER_BOUND('',#1367,.T.);
#954=FACE_OUTER_BOUND('',#1368,.T.);
#955=FACE_OUTER_BOUND('',#1369,.T.);
#956=FACE_OUTER_BOUND('',#1370,.T.);
#957=FACE_OUTER_BOUND('',#1371,.T.);
#958=FACE_OUTER_BOUND('',#1372,.T.);
#959=FACE_OUTER_BOUND('',#1373,.T.);
#960=FACE_OUTER_BOUND('',#1374,.T.);
#961=FACE_OUTER_BOUND('',#1375,.T.);
#962=FACE_OUTER_BOUND('',#1382,.T.);
#963=FACE_OUTER_BOUND('',#1383,.T.);
#964=FACE_OUTER_BOUND('',#1384,.T.);
#965=FACE_OUTER_BOUND('',#1388,.T.);
#966=FACE_OUTER_BOUND('',#1389,.T.);
#967=FACE_OUTER_BOUND('',#1390,.T.);
#968=FACE_OUTER_BOUND('',#1391,.T.);
#969=FACE_OUTER_BOUND('',#1392,.T.);
#970=FACE_OUTER_BOUND('',#1393,.T.);
#971=FACE_OUTER_BOUND('',#1394,.T.);
#972=FACE_OUTER_BOUND('',#1395,.T.);
#973=FACE_OUTER_BOUND('',#1396,.T.);
#974=FACE_OUTER_BOUND('',#1397,.T.);
#975=FACE_OUTER_BOUND('',#1398,.T.);
#976=FACE_OUTER_BOUND('',#1400,.T.);
#977=FACE_OUTER_BOUND('',#1401,.T.);
#978=FACE_OUTER_BOUND('',#1402,.T.);
#979=FACE_OUTER_BOUND('',#1403,.T.);
#980=FACE_OUTER_BOUND('',#1404,.T.);
#981=FACE_OUTER_BOUND('',#1405,.T.);
#982=FACE_OUTER_BOUND('',#1406,.T.);
#983=FACE_OUTER_BOUND('',#1408,.T.);
#984=FACE_OUTER_BOUND('',#1409,.T.);
#985=FACE_OUTER_BOUND('',#1410,.T.);
#986=FACE_OUTER_BOUND('',#1411,.T.);
#987=FACE_OUTER_BOUND('',#1412,.T.);
#988=FACE_OUTER_BOUND('',#1413,.T.);
#989=FACE_OUTER_BOUND('',#1414,.T.);
#990=FACE_OUTER_BOUND('',#1415,.T.);
#991=FACE_OUTER_BOUND('',#1416,.T.);
#992=FACE_OUTER_BOUND('',#1417,.T.);
#993=FACE_OUTER_BOUND('',#1419,.T.);
#994=FACE_OUTER_BOUND('',#1421,.T.);
#995=FACE_OUTER_BOUND('',#1422,.T.);
#996=FACE_OUTER_BOUND('',#1423,.T.);
#997=FACE_OUTER_BOUND('',#1424,.T.);
#998=FACE_OUTER_BOUND('',#1425,.T.);
#999=FACE_OUTER_BOUND('',#1426,.T.);
#1000=FACE_OUTER_BOUND('',#1427,.T.);
#1001=FACE_OUTER_BOUND('',#1428,.T.);
#1002=FACE_OUTER_BOUND('',#1429,.T.);
#1003=FACE_OUTER_BOUND('',#1430,.T.);
#1004=FACE_OUTER_BOUND('',#1431,.T.);
#1005=FACE_OUTER_BOUND('',#1433,.T.);
#1006=FACE_OUTER_BOUND('',#1434,.T.);
#1007=FACE_OUTER_BOUND('',#1435,.T.);
#1008=FACE_OUTER_BOUND('',#1436,.T.);
#1009=FACE_OUTER_BOUND('',#1437,.T.);
#1010=FACE_OUTER_BOUND('',#1438,.T.);
#1011=FACE_OUTER_BOUND('',#1439,.T.);
#1012=FACE_OUTER_BOUND('',#1440,.T.);
#1013=FACE_OUTER_BOUND('',#1444,.T.);
#1014=FACE_OUTER_BOUND('',#1445,.T.);
#1015=FACE_OUTER_BOUND('',#1446,.T.);
#1016=FACE_OUTER_BOUND('',#1447,.T.);
#1017=FACE_OUTER_BOUND('',#1448,.T.);
#1018=FACE_OUTER_BOUND('',#1449,.T.);
#1019=FACE_OUTER_BOUND('',#1450,.T.);
#1020=FACE_OUTER_BOUND('',#1451,.T.);
#1021=FACE_OUTER_BOUND('',#1452,.T.);
#1022=FACE_OUTER_BOUND('',#1453,.T.);
#1023=FACE_OUTER_BOUND('',#1454,.T.);
#1024=FACE_OUTER_BOUND('',#1455,.T.);
#1025=FACE_OUTER_BOUND('',#1456,.T.);
#1026=FACE_OUTER_BOUND('',#1457,.T.);
#1027=FACE_OUTER_BOUND('',#1458,.T.);
#1028=FACE_OUTER_BOUND('',#1459,.T.);
#1029=FACE_OUTER_BOUND('',#1460,.T.);
#1030=FACE_OUTER_BOUND('',#1461,.T.);
#1031=FACE_OUTER_BOUND('',#1462,.T.);
#1032=FACE_OUTER_BOUND('',#1463,.T.);
#1033=FACE_OUTER_BOUND('',#1464,.T.);
#1034=FACE_OUTER_BOUND('',#1465,.T.);
#1035=FACE_OUTER_BOUND('',#1466,.T.);
#1036=FACE_OUTER_BOUND('',#1467,.T.);
#1037=FACE_OUTER_BOUND('',#1468,.T.);
#1038=FACE_OUTER_BOUND('',#1469,.T.);
#1039=FACE_OUTER_BOUND('',#1470,.T.);
#1040=FACE_OUTER_BOUND('',#1471,.T.);
#1041=FACE_OUTER_BOUND('',#1472,.T.);
#1042=FACE_OUTER_BOUND('',#1473,.T.);
#1043=FACE_OUTER_BOUND('',#1474,.T.);
#1044=FACE_OUTER_BOUND('',#1475,.T.);
#1045=FACE_OUTER_BOUND('',#1476,.T.);
#1046=FACE_OUTER_BOUND('',#1477,.T.);
#1047=FACE_OUTER_BOUND('',#1478,.T.);
#1048=FACE_OUTER_BOUND('',#1479,.T.);
#1049=FACE_OUTER_BOUND('',#1480,.T.);
#1050=FACE_OUTER_BOUND('',#1481,.T.);
#1051=FACE_OUTER_BOUND('',#1482,.T.);
#1052=FACE_OUTER_BOUND('',#1483,.T.);
#1053=FACE_OUTER_BOUND('',#1484,.T.);
#1054=FACE_OUTER_BOUND('',#1485,.T.);
#1055=FACE_OUTER_BOUND('',#1486,.T.);
#1056=FACE_OUTER_BOUND('',#1487,.T.);
#1057=FACE_OUTER_BOUND('',#1488,.T.);
#1058=FACE_OUTER_BOUND('',#1489,.T.);
#1059=FACE_OUTER_BOUND('',#1490,.T.);
#1060=FACE_OUTER_BOUND('',#1491,.T.);
#1061=FACE_OUTER_BOUND('',#1498,.T.);
#1062=FACE_OUTER_BOUND('',#1499,.T.);
#1063=FACE_OUTER_BOUND('',#1500,.T.);
#1064=FACE_OUTER_BOUND('',#1501,.T.);
#1065=FACE_OUTER_BOUND('',#1502,.T.);
#1066=FACE_OUTER_BOUND('',#1504,.T.);
#1067=FACE_OUTER_BOUND('',#1505,.T.);
#1068=FACE_OUTER_BOUND('',#1506,.T.);
#1069=FACE_OUTER_BOUND('',#1508,.T.);
#1070=FACE_OUTER_BOUND('',#1509,.T.);
#1071=FACE_OUTER_BOUND('',#1510,.T.);
#1072=FACE_OUTER_BOUND('',#1512,.T.);
#1073=FACE_OUTER_BOUND('',#1513,.T.);
#1074=FACE_OUTER_BOUND('',#1514,.T.);
#1075=FACE_OUTER_BOUND('',#1516,.T.);
#1076=FACE_OUTER_BOUND('',#1517,.T.);
#1077=FACE_OUTER_BOUND('',#1518,.T.);
#1078=FACE_OUTER_BOUND('',#1519,.T.);
#1079=FACE_OUTER_BOUND('',#1520,.T.);
#1080=FACE_OUTER_BOUND('',#1521,.T.);
#1081=FACE_OUTER_BOUND('',#1522,.T.);
#1082=FACE_OUTER_BOUND('',#1523,.T.);
#1083=FACE_OUTER_BOUND('',#1524,.T.);
#1084=FACE_OUTER_BOUND('',#1525,.T.);
#1085=FACE_OUTER_BOUND('',#1526,.T.);
#1086=FACE_OUTER_BOUND('',#1527,.T.);
#1087=FACE_OUTER_BOUND('',#1528,.T.);
#1088=FACE_OUTER_BOUND('',#1529,.T.);
#1089=FACE_OUTER_BOUND('',#1530,.T.);
#1090=FACE_OUTER_BOUND('',#1531,.T.);
#1091=FACE_OUTER_BOUND('',#1532,.T.);
#1092=FACE_OUTER_BOUND('',#1533,.T.);
#1093=FACE_OUTER_BOUND('',#1534,.T.);
#1094=FACE_OUTER_BOUND('',#1537,.T.);
#1095=FACE_OUTER_BOUND('',#1538,.T.);
#1096=FACE_OUTER_BOUND('',#1539,.T.);
#1097=FACE_OUTER_BOUND('',#1540,.T.);
#1098=FACE_OUTER_BOUND('',#1547,.T.);
#1099=FACE_OUTER_BOUND('',#1548,.T.);
#1100=FACE_OUTER_BOUND('',#1549,.T.);
#1101=FACE_OUTER_BOUND('',#1550,.T.);
#1102=FACE_OUTER_BOUND('',#1551,.T.);
#1103=FACE_OUTER_BOUND('',#1552,.T.);
#1104=FACE_OUTER_BOUND('',#1553,.T.);
#1105=FACE_OUTER_BOUND('',#1554,.T.);
#1106=FACE_OUTER_BOUND('',#1555,.T.);
#1107=FACE_OUTER_BOUND('',#1556,.T.);
#1108=FACE_OUTER_BOUND('',#1557,.T.);
#1109=FACE_OUTER_BOUND('',#1558,.T.);
#1110=FACE_OUTER_BOUND('',#1559,.T.);
#1111=FACE_OUTER_BOUND('',#1560,.T.);
#1112=FACE_OUTER_BOUND('',#1561,.T.);
#1113=FACE_OUTER_BOUND('',#1562,.T.);
#1114=FACE_OUTER_BOUND('',#1563,.T.);
#1115=FACE_OUTER_BOUND('',#1564,.T.);
#1116=FACE_OUTER_BOUND('',#1565,.T.);
#1117=FACE_OUTER_BOUND('',#1566,.T.);
#1118=FACE_OUTER_BOUND('',#1567,.T.);
#1119=FACE_OUTER_BOUND('',#1568,.T.);
#1120=FACE_OUTER_BOUND('',#1569,.T.);
#1121=FACE_OUTER_BOUND('',#1570,.T.);
#1122=FACE_OUTER_BOUND('',#1571,.T.);
#1123=FACE_OUTER_BOUND('',#1572,.T.);
#1124=FACE_OUTER_BOUND('',#1573,.T.);
#1125=FACE_OUTER_BOUND('',#1574,.T.);
#1126=FACE_OUTER_BOUND('',#1575,.T.);
#1127=FACE_OUTER_BOUND('',#1576,.T.);
#1128=FACE_OUTER_BOUND('',#1577,.T.);
#1129=FACE_OUTER_BOUND('',#1578,.T.);
#1130=FACE_OUTER_BOUND('',#1579,.T.);
#1131=FACE_OUTER_BOUND('',#1580,.T.);
#1132=FACE_OUTER_BOUND('',#1581,.T.);
#1133=FACE_OUTER_BOUND('',#1582,.T.);
#1134=FACE_OUTER_BOUND('',#1583,.T.);
#1135=FACE_OUTER_BOUND('',#1584,.T.);
#1136=FACE_OUTER_BOUND('',#1585,.T.);
#1137=FACE_OUTER_BOUND('',#1586,.T.);
#1138=FACE_OUTER_BOUND('',#1587,.T.);
#1139=FACE_OUTER_BOUND('',#1588,.T.);
#1140=FACE_OUTER_BOUND('',#1589,.T.);
#1141=FACE_OUTER_BOUND('',#1590,.T.);
#1142=FACE_OUTER_BOUND('',#1591,.T.);
#1143=FACE_OUTER_BOUND('',#1592,.T.);
#1144=FACE_OUTER_BOUND('',#1593,.T.);
#1145=FACE_OUTER_BOUND('',#1594,.T.);
#1146=FACE_OUTER_BOUND('',#1595,.T.);
#1147=FACE_OUTER_BOUND('',#1596,.T.);
#1148=FACE_OUTER_BOUND('',#1597,.T.);
#1149=FACE_OUTER_BOUND('',#1598,.T.);
#1150=FACE_OUTER_BOUND('',#1599,.T.);
#1151=FACE_OUTER_BOUND('',#1600,.T.);
#1152=FACE_OUTER_BOUND('',#1601,.T.);
#1153=FACE_OUTER_BOUND('',#1602,.T.);
#1154=FACE_OUTER_BOUND('',#1603,.T.);
#1155=FACE_OUTER_BOUND('',#1604,.T.);
#1156=FACE_OUTER_BOUND('',#1605,.T.);
#1157=FACE_OUTER_BOUND('',#1606,.T.);
#1158=FACE_OUTER_BOUND('',#1607,.T.);
#1159=FACE_OUTER_BOUND('',#1608,.T.);
#1160=FACE_OUTER_BOUND('',#1609,.T.);
#1161=FACE_OUTER_BOUND('',#1610,.T.);
#1162=FACE_OUTER_BOUND('',#1611,.T.);
#1163=FACE_OUTER_BOUND('',#1612,.T.);
#1164=FACE_OUTER_BOUND('',#1613,.T.);
#1165=FACE_OUTER_BOUND('',#1614,.T.);
#1166=FACE_OUTER_BOUND('',#1615,.T.);
#1167=FACE_OUTER_BOUND('',#1616,.T.);
#1168=FACE_OUTER_BOUND('',#1617,.T.);
#1169=FACE_OUTER_BOUND('',#1618,.T.);
#1170=FACE_OUTER_BOUND('',#1619,.T.);
#1171=FACE_OUTER_BOUND('',#1620,.T.);
#1172=FACE_OUTER_BOUND('',#1622,.T.);
#1173=FACE_OUTER_BOUND('',#1623,.T.);
#1174=FACE_OUTER_BOUND('',#1625,.T.);
#1175=FACE_OUTER_BOUND('',#1626,.T.);
#1176=FACE_OUTER_BOUND('',#1627,.T.);
#1177=FACE_OUTER_BOUND('',#1628,.T.);
#1178=FACE_OUTER_BOUND('',#1629,.T.);
#1179=FACE_OUTER_BOUND('',#1630,.T.);
#1180=FACE_OUTER_BOUND('',#1631,.T.);
#1181=FACE_OUTER_BOUND('',#1632,.T.);
#1182=FACE_OUTER_BOUND('',#1633,.T.);
#1183=FACE_OUTER_BOUND('',#1634,.T.);
#1184=FACE_OUTER_BOUND('',#1635,.T.);
#1185=FACE_OUTER_BOUND('',#1636,.T.);
#1186=FACE_OUTER_BOUND('',#1637,.T.);
#1187=FACE_OUTER_BOUND('',#1638,.T.);
#1188=FACE_OUTER_BOUND('',#1639,.T.);
#1189=FACE_OUTER_BOUND('',#1641,.T.);
#1190=FACE_OUTER_BOUND('',#1642,.T.);
#1191=FACE_OUTER_BOUND('',#1643,.T.);
#1192=FACE_OUTER_BOUND('',#1644,.T.);
#1193=FACE_OUTER_BOUND('',#1645,.T.);
#1194=FACE_OUTER_BOUND('',#1646,.T.);
#1195=FACE_OUTER_BOUND('',#1647,.T.);
#1196=FACE_OUTER_BOUND('',#1648,.T.);
#1197=FACE_OUTER_BOUND('',#1650,.T.);
#1198=FACE_OUTER_BOUND('',#1651,.T.);
#1199=FACE_OUTER_BOUND('',#1652,.T.);
#1200=FACE_OUTER_BOUND('',#1654,.T.);
#1201=EDGE_LOOP('',(#4335,#4336,#4337,#4338));
#1202=EDGE_LOOP('',(#4339,#4340,#4341,#4342));
#1203=EDGE_LOOP('',(#4343,#4344,#4345,#4346));
#1204=EDGE_LOOP('',(#4347,#4348,#4349));
#1205=EDGE_LOOP('',(#4350,#4351,#4352,#4353));
#1206=EDGE_LOOP('',(#4354,#4355,#4356));
#1207=EDGE_LOOP('',(#4357,#4358,#4359,#4360,#4361,#4362,#4363));
#1208=EDGE_LOOP('',(#4364,#4365,#4366));
#1209=EDGE_LOOP('',(#4367,#4368,#4369,#4370));
#1210=EDGE_LOOP('',(#4371,#4372,#4373));
#1211=EDGE_LOOP('',(#4374,#4375,#4376,#4377,#4378,#4379,#4380,#4381,#4382,
#4383,#4384,#4385,#4386,#4387,#4388,#4389,#4390));
#1212=EDGE_LOOP('',(#4391));
#1213=EDGE_LOOP('',(#4392));
#1214=EDGE_LOOP('',(#4393));
#1215=EDGE_LOOP('',(#4394,#4395,#4396,#4397));
#1216=EDGE_LOOP('',(#4398,#4399,#4400,#4401,#4402,#4403,#4404,#4405,#4406));
#1217=EDGE_LOOP('',(#4407,#4408,#4409,#4410,#4411));
#1218=EDGE_LOOP('',(#4412,#4413,#4414,#4415));
#1219=EDGE_LOOP('',(#4416,#4417,#4418,#4419));
#1220=EDGE_LOOP('',(#4420,#4421,#4422,#4423));
#1221=EDGE_LOOP('',(#4424,#4425,#4426,#4427,#4428,#4429));
#1222=EDGE_LOOP('',(#4430,#4431,#4432,#4433,#4434,#4435,#4436,#4437,#4438,
#4439,#4440,#4441));
#1223=EDGE_LOOP('',(#4442));
#1224=EDGE_LOOP('',(#4443));
#1225=EDGE_LOOP('',(#4444));
#1226=EDGE_LOOP('',(#4445,#4446,#4447,#4448));
#1227=EDGE_LOOP('',(#4449,#4450,#4451,#4452));
#1228=EDGE_LOOP('',(#4453,#4454,#4455,#4456));
#1229=EDGE_LOOP('',(#4457,#4458,#4459,#4460));
#1230=EDGE_LOOP('',(#4461,#4462,#4463,#4464));
#1231=EDGE_LOOP('',(#4465,#4466,#4467,#4468));
#1232=EDGE_LOOP('',(#4469,#4470,#4471,#4472));
#1233=EDGE_LOOP('',(#4473,#4474,#4475,#4476));
#1234=EDGE_LOOP('',(#4477,#4478,#4479,#4480));
#1235=EDGE_LOOP('',(#4481,#4482,#4483,#4484));
#1236=EDGE_LOOP('',(#4485,#4486,#4487,#4488));
#1237=EDGE_LOOP('',(#4489,#4490,#4491,#4492));
#1238=EDGE_LOOP('',(#4493,#4494,#4495,#4496,#4497));
#1239=EDGE_LOOP('',(#4498,#4499,#4500,#4501,#4502,#4503));
#1240=EDGE_LOOP('',(#4504,#4505,#4506,#4507));
#1241=EDGE_LOOP('',(#4508,#4509,#4510,#4511));
#1242=EDGE_LOOP('',(#4512,#4513,#4514,#4515));
#1243=EDGE_LOOP('',(#4516,#4517,#4518,#4519,#4520,#4521));
#1244=EDGE_LOOP('',(#4522,#4523,#4524,#4525,#4526,#4527,#4528,#4529,#4530,
#4531,#4532,#4533));
#1245=EDGE_LOOP('',(#4534));
#1246=EDGE_LOOP('',(#4535));
#1247=EDGE_LOOP('',(#4536));
#1248=EDGE_LOOP('',(#4537,#4538,#4539,#4540));
#1249=EDGE_LOOP('',(#4541,#4542,#4543,#4544));
#1250=EDGE_LOOP('',(#4545,#4546,#4547,#4548));
#1251=EDGE_LOOP('',(#4549,#4550,#4551,#4552));
#1252=EDGE_LOOP('',(#4553,#4554,#4555,#4556));
#1253=EDGE_LOOP('',(#4557,#4558,#4559,#4560));
#1254=EDGE_LOOP('',(#4561,#4562,#4563,#4564));
#1255=EDGE_LOOP('',(#4565,#4566,#4567,#4568,#4569,#4570,#4571,#4572,#4573,
#4574,#4575,#4576,#4577));
#1256=EDGE_LOOP('',(#4578));
#1257=EDGE_LOOP('',(#4579));
#1258=EDGE_LOOP('',(#4580));
#1259=EDGE_LOOP('',(#4581,#4582,#4583,#4584));
#1260=EDGE_LOOP('',(#4585,#4586,#4587,#4588));
#1261=EDGE_LOOP('',(#4589));
#1262=EDGE_LOOP('',(#4590));
#1263=EDGE_LOOP('',(#4591));
#1264=EDGE_LOOP('',(#4592));
#1265=EDGE_LOOP('',(#4593,#4594,#4595,#4596));
#1266=EDGE_LOOP('',(#4597));
#1267=EDGE_LOOP('',(#4598));
#1268=EDGE_LOOP('',(#4599,#4600,#4601,#4602));
#1269=EDGE_LOOP('',(#4603));
#1270=EDGE_LOOP('',(#4604,#4605,#4606,#4607));
#1271=EDGE_LOOP('',(#4608));
#1272=EDGE_LOOP('',(#4609,#4610,#4611,#4612));
#1273=EDGE_LOOP('',(#4613,#4614,#4615,#4616));
#1274=EDGE_LOOP('',(#4617,#4618,#4619,#4620));
#1275=EDGE_LOOP('',(#4621,#4622,#4623,#4624));
#1276=EDGE_LOOP('',(#4625,#4626,#4627,#4628));
#1277=EDGE_LOOP('',(#4629,#4630,#4631,#4632));
#1278=EDGE_LOOP('',(#4633,#4634,#4635,#4636,#4637,#4638,#4639,#4640));
#1279=EDGE_LOOP('',(#4641));
#1280=EDGE_LOOP('',(#4642));
#1281=EDGE_LOOP('',(#4643));
#1282=EDGE_LOOP('',(#4644,#4645,#4646,#4647));
#1283=EDGE_LOOP('',(#4648,#4649,#4650,#4651));
#1284=EDGE_LOOP('',(#4652,#4653,#4654,#4655));
#1285=EDGE_LOOP('',(#4656,#4657,#4658,#4659));
#1286=EDGE_LOOP('',(#4660,#4661,#4662,#4663));
#1287=EDGE_LOOP('',(#4664));
#1288=EDGE_LOOP('',(#4665));
#1289=EDGE_LOOP('',(#4666,#4667,#4668,#4669));
#1290=EDGE_LOOP('',(#4670));
#1291=EDGE_LOOP('',(#4671));
#1292=EDGE_LOOP('',(#4672,#4673,#4674,#4675));
#1293=EDGE_LOOP('',(#4676,#4677,#4678,#4679));
#1294=EDGE_LOOP('',(#4680,#4681,#4682,#4683));
#1295=EDGE_LOOP('',(#4684,#4685,#4686,#4687));
#1296=EDGE_LOOP('',(#4688,#4689,#4690,#4691));
#1297=EDGE_LOOP('',(#4692,#4693,#4694,#4695));
#1298=EDGE_LOOP('',(#4696,#4697,#4698,#4699));
#1299=EDGE_LOOP('',(#4700,#4701,#4702,#4703));
#1300=EDGE_LOOP('',(#4704,#4705,#4706,#4707));
#1301=EDGE_LOOP('',(#4708));
#1302=EDGE_LOOP('',(#4709));
#1303=EDGE_LOOP('',(#4710));
#1304=EDGE_LOOP('',(#4711));
#1305=EDGE_LOOP('',(#4712,#4713,#4714,#4715));
#1306=EDGE_LOOP('',(#4716,#4717,#4718,#4719));
#1307=EDGE_LOOP('',(#4720,#4721,#4722,#4723));
#1308=EDGE_LOOP('',(#4724,#4725,#4726,#4727));
#1309=EDGE_LOOP('',(#4728,#4729,#4730,#4731));
#1310=EDGE_LOOP('',(#4732,#4733,#4734,#4735,#4736,#4737));
#1311=EDGE_LOOP('',(#4738,#4739,#4740,#4741,#4742,#4743,#4744,#4745,#4746,
#4747));
#1312=EDGE_LOOP('',(#4748,#4749,#4750,#4751,#4752,#4753,#4754,#4755,#4756,
#4757));
#1313=EDGE_LOOP('',(#4758,#4759,#4760,#4761,#4762,#4763,#4764,#4765,#4766,
#4767));
#1314=EDGE_LOOP('',(#4768,#4769,#4770,#4771,#4772,#4773,#4774,#4775));
#1315=EDGE_LOOP('',(#4776,#4777,#4778,#4779,#4780,#4781,#4782,#4783,#4784,
#4785,#4786,#4787,#4788,#4789,#4790,#4791,#4792,#4793,#4794,#4795,#4796,
#4797,#4798,#4799,#4800,#4801,#4802,#4803,#4804,#4805,#4806,#4807,#4808,
#4809,#4810,#4811,#4812,#4813,#4814,#4815,#4816,#4817));
#1316=EDGE_LOOP('',(#4818,#4819,#4820,#4821,#4822,#4823));
#1317=EDGE_LOOP('',(#4824,#4825,#4826,#4827));
#1318=EDGE_LOOP('',(#4828,#4829,#4830,#4831));
#1319=EDGE_LOOP('',(#4832,#4833,#4834,#4835,#4836,#4837));
#1320=EDGE_LOOP('',(#4838,#4839,#4840,#4841));
#1321=EDGE_LOOP('',(#4842,#4843,#4844,#4845));
#1322=EDGE_LOOP('',(#4846,#4847,#4848,#4849));
#1323=EDGE_LOOP('',(#4850,#4851,#4852,#4853));
#1324=EDGE_LOOP('',(#4854,#4855,#4856,#4857));
#1325=EDGE_LOOP('',(#4858));
#1326=EDGE_LOOP('',(#4859));
#1327=EDGE_LOOP('',(#4860));
#1328=EDGE_LOOP('',(#4861,#4862,#4863,#4864));
#1329=EDGE_LOOP('',(#4865,#4866,#4867,#4868));
#1330=EDGE_LOOP('',(#4869,#4870,#4871,#4872));
#1331=EDGE_LOOP('',(#4873,#4874,#4875,#4876));
#1332=EDGE_LOOP('',(#4877,#4878,#4879,#4880,#4881,#4882,#4883,#4884,#4885,
#4886));
#1333=EDGE_LOOP('',(#4887,#4888,#4889,#4890));
#1334=EDGE_LOOP('',(#4891,#4892,#4893,#4894));
#1335=EDGE_LOOP('',(#4895,#4896,#4897,#4898));
#1336=EDGE_LOOP('',(#4899,#4900,#4901,#4902));
#1337=EDGE_LOOP('',(#4903,#4904,#4905,#4906));
#1338=EDGE_LOOP('',(#4907,#4908,#4909,#4910,#4911,#4912,#4913,#4914,#4915,
#4916));
#1339=EDGE_LOOP('',(#4917,#4918,#4919,#4920));
#1340=EDGE_LOOP('',(#4921,#4922,#4923,#4924,#4925,#4926));
#1341=EDGE_LOOP('',(#4927,#4928,#4929,#4930,#4931,#4932));
#1342=EDGE_LOOP('',(#4933,#4934,#4935,#4936));
#1343=EDGE_LOOP('',(#4937,#4938,#4939,#4940,#4941,#4942,#4943,#4944,#4945,
#4946));
#1344=EDGE_LOOP('',(#4947,#4948,#4949,#4950));
#1345=EDGE_LOOP('',(#4951,#4952,#4953,#4954));
#1346=EDGE_LOOP('',(#4955,#4956,#4957,#4958));
#1347=EDGE_LOOP('',(#4959,#4960,#4961,#4962));
#1348=EDGE_LOOP('',(#4963,#4964,#4965,#4966));
#1349=EDGE_LOOP('',(#4967,#4968,#4969));
#1350=EDGE_LOOP('',(#4970,#4971,#4972));
#1351=EDGE_LOOP('',(#4973,#4974,#4975));
#1352=EDGE_LOOP('',(#4976,#4977,#4978,#4979));
#1353=EDGE_LOOP('',(#4980,#4981,#4982,#4983));
#1354=EDGE_LOOP('',(#4984,#4985,#4986));
#1355=EDGE_LOOP('',(#4987,#4988,#4989,#4990));
#1356=EDGE_LOOP('',(#4991,#4992,#4993,#4994));
#1357=EDGE_LOOP('',(#4995,#4996,#4997,#4998));
#1358=EDGE_LOOP('',(#4999,#5000,#5001,#5002));
#1359=EDGE_LOOP('',(#5003,#5004,#5005,#5006));
#1360=EDGE_LOOP('',(#5007,#5008,#5009,#5010));
#1361=EDGE_LOOP('',(#5011,#5012,#5013));
#1362=EDGE_LOOP('',(#5014,#5015,#5016));
#1363=EDGE_LOOP('',(#5017,#5018,#5019));
#1364=EDGE_LOOP('',(#5020,#5021,#5022,#5023));
#1365=EDGE_LOOP('',(#5024,#5025,#5026,#5027));
#1366=EDGE_LOOP('',(#5028,#5029,#5030));
#1367=EDGE_LOOP('',(#5031,#5032,#5033,#5034));
#1368=EDGE_LOOP('',(#5035,#5036,#5037,#5038));
#1369=EDGE_LOOP('',(#5039,#5040,#5041,#5042));
#1370=EDGE_LOOP('',(#5043,#5044,#5045,#5046));
#1371=EDGE_LOOP('',(#5047,#5048,#5049,#5050));
#1372=EDGE_LOOP('',(#5051,#5052,#5053,#5054));
#1373=EDGE_LOOP('',(#5055,#5056,#5057,#5058));
#1374=EDGE_LOOP('',(#5059,#5060,#5061,#5062,#5063,#5064,#5065,#5066));
#1375=EDGE_LOOP('',(#5067,#5068,#5069,#5070));
#1376=EDGE_LOOP('',(#5071));
#1377=EDGE_LOOP('',(#5072));
#1378=EDGE_LOOP('',(#5073));
#1379=EDGE_LOOP('',(#5074));
#1380=EDGE_LOOP('',(#5075));
#1381=EDGE_LOOP('',(#5076));
#1382=EDGE_LOOP('',(#5077,#5078,#5079,#5080));
#1383=EDGE_LOOP('',(#5081,#5082,#5083,#5084));
#1384=EDGE_LOOP('',(#5085,#5086,#5087,#5088,#5089,#5090,#5091,#5092));
#1385=EDGE_LOOP('',(#5093));
#1386=EDGE_LOOP('',(#5094));
#1387=EDGE_LOOP('',(#5095));
#1388=EDGE_LOOP('',(#5096,#5097,#5098,#5099));
#1389=EDGE_LOOP('',(#5100,#5101,#5102,#5103));
#1390=EDGE_LOOP('',(#5104,#5105,#5106,#5107));
#1391=EDGE_LOOP('',(#5108,#5109,#5110,#5111));
#1392=EDGE_LOOP('',(#5112,#5113,#5114,#5115));
#1393=EDGE_LOOP('',(#5116,#5117,#5118,#5119));
#1394=EDGE_LOOP('',(#5120,#5121,#5122,#5123));
#1395=EDGE_LOOP('',(#5124,#5125,#5126,#5127));
#1396=EDGE_LOOP('',(#5128,#5129,#5130,#5131));
#1397=EDGE_LOOP('',(#5132,#5133,#5134,#5135));
#1398=EDGE_LOOP('',(#5136,#5137,#5138,#5139,#5140,#5141));
#1399=EDGE_LOOP('',(#5142));
#1400=EDGE_LOOP('',(#5143,#5144,#5145,#5146));
#1401=EDGE_LOOP('',(#5147,#5148,#5149,#5150));
#1402=EDGE_LOOP('',(#5151,#5152,#5153,#5154));
#1403=EDGE_LOOP('',(#5155,#5156,#5157,#5158));
#1404=EDGE_LOOP('',(#5159,#5160,#5161,#5162));
#1405=EDGE_LOOP('',(#5163,#5164,#5165,#5166));
#1406=EDGE_LOOP('',(#5167,#5168,#5169,#5170,#5171,#5172));
#1407=EDGE_LOOP('',(#5173));
#1408=EDGE_LOOP('',(#5174,#5175,#5176,#5177));
#1409=EDGE_LOOP('',(#5178,#5179,#5180,#5181));
#1410=EDGE_LOOP('',(#5182,#5183,#5184,#5185));
#1411=EDGE_LOOP('',(#5186,#5187,#5188,#5189));
#1412=EDGE_LOOP('',(#5190,#5191,#5192,#5193));
#1413=EDGE_LOOP('',(#5194,#5195,#5196,#5197));
#1414=EDGE_LOOP('',(#5198,#5199,#5200,#5201));
#1415=EDGE_LOOP('',(#5202,#5203,#5204,#5205));
#1416=EDGE_LOOP('',(#5206,#5207,#5208,#5209));
#1417=EDGE_LOOP('',(#5210));
#1418=EDGE_LOOP('',(#5211));
#1419=EDGE_LOOP('',(#5212));
#1420=EDGE_LOOP('',(#5213));
#1421=EDGE_LOOP('',(#5214,#5215,#5216,#5217));
#1422=EDGE_LOOP('',(#5218,#5219,#5220,#5221));
#1423=EDGE_LOOP('',(#5222,#5223,#5224,#5225));
#1424=EDGE_LOOP('',(#5226,#5227,#5228,#5229));
#1425=EDGE_LOOP('',(#5230,#5231,#5232,#5233));
#1426=EDGE_LOOP('',(#5234,#5235,#5236,#5237,#5238,#5239));
#1427=EDGE_LOOP('',(#5240,#5241,#5242,#5243,#5244,#5245,#5246,#5247,#5248,
#5249));
#1428=EDGE_LOOP('',(#5250,#5251,#5252,#5253,#5254,#5255,#5256,#5257,#5258,
#5259));
#1429=EDGE_LOOP('',(#5260,#5261,#5262,#5263,#5264,#5265,#5266,#5267,#5268,
#5269));
#1430=EDGE_LOOP('',(#5270,#5271,#5272,#5273,#5274,#5275,#5276,#5277));
#1431=EDGE_LOOP('',(#5278,#5279,#5280,#5281,#5282,#5283,#5284,#5285,#5286,
#5287,#5288,#5289,#5290,#5291,#5292,#5293,#5294,#5295,#5296,#5297,#5298,
#5299,#5300,#5301,#5302,#5303,#5304,#5305,#5306,#5307,#5308,#5309,#5310,
#5311,#5312,#5313,#5314,#5315,#5316,#5317,#5318,#5319));
#1432=EDGE_LOOP('',(#5320,#5321,#5322,#5323,#5324,#5325));
#1433=EDGE_LOOP('',(#5326,#5327,#5328,#5329));
#1434=EDGE_LOOP('',(#5330,#5331,#5332,#5333));
#1435=EDGE_LOOP('',(#5334,#5335,#5336,#5337,#5338,#5339));
#1436=EDGE_LOOP('',(#5340,#5341,#5342,#5343));
#1437=EDGE_LOOP('',(#5344,#5345,#5346,#5347));
#1438=EDGE_LOOP('',(#5348,#5349,#5350,#5351));
#1439=EDGE_LOOP('',(#5352,#5353,#5354,#5355));
#1440=EDGE_LOOP('',(#5356,#5357,#5358,#5359));
#1441=EDGE_LOOP('',(#5360));
#1442=EDGE_LOOP('',(#5361));
#1443=EDGE_LOOP('',(#5362));
#1444=EDGE_LOOP('',(#5363,#5364,#5365,#5366));
#1445=EDGE_LOOP('',(#5367,#5368,#5369,#5370));
#1446=EDGE_LOOP('',(#5371,#5372,#5373,#5374));
#1447=EDGE_LOOP('',(#5375,#5376,#5377,#5378));
#1448=EDGE_LOOP('',(#5379,#5380,#5381,#5382,#5383,#5384,#5385,#5386,#5387,
#5388));
#1449=EDGE_LOOP('',(#5389,#5390,#5391,#5392));
#1450=EDGE_LOOP('',(#5393,#5394,#5395,#5396));
#1451=EDGE_LOOP('',(#5397,#5398,#5399,#5400));
#1452=EDGE_LOOP('',(#5401,#5402,#5403,#5404));
#1453=EDGE_LOOP('',(#5405,#5406,#5407,#5408));
#1454=EDGE_LOOP('',(#5409,#5410,#5411,#5412,#5413,#5414,#5415,#5416,#5417,
#5418));
#1455=EDGE_LOOP('',(#5419,#5420,#5421,#5422));
#1456=EDGE_LOOP('',(#5423,#5424,#5425,#5426,#5427,#5428));
#1457=EDGE_LOOP('',(#5429,#5430,#5431,#5432,#5433,#5434));
#1458=EDGE_LOOP('',(#5435,#5436,#5437,#5438));
#1459=EDGE_LOOP('',(#5439,#5440,#5441,#5442,#5443,#5444,#5445,#5446,#5447,
#5448));
#1460=EDGE_LOOP('',(#5449,#5450,#5451,#5452));
#1461=EDGE_LOOP('',(#5453,#5454,#5455,#5456));
#1462=EDGE_LOOP('',(#5457,#5458,#5459,#5460));
#1463=EDGE_LOOP('',(#5461,#5462,#5463,#5464));
#1464=EDGE_LOOP('',(#5465,#5466,#5467,#5468));
#1465=EDGE_LOOP('',(#5469,#5470,#5471));
#1466=EDGE_LOOP('',(#5472,#5473,#5474));
#1467=EDGE_LOOP('',(#5475,#5476,#5477));
#1468=EDGE_LOOP('',(#5478,#5479,#5480,#5481));
#1469=EDGE_LOOP('',(#5482,#5483,#5484,#5485));
#1470=EDGE_LOOP('',(#5486,#5487,#5488));
#1471=EDGE_LOOP('',(#5489,#5490,#5491,#5492));
#1472=EDGE_LOOP('',(#5493,#5494,#5495,#5496));
#1473=EDGE_LOOP('',(#5497,#5498,#5499,#5500));
#1474=EDGE_LOOP('',(#5501,#5502,#5503,#5504));
#1475=EDGE_LOOP('',(#5505,#5506,#5507,#5508));
#1476=EDGE_LOOP('',(#5509,#5510,#5511,#5512));
#1477=EDGE_LOOP('',(#5513,#5514,#5515));
#1478=EDGE_LOOP('',(#5516,#5517,#5518));
#1479=EDGE_LOOP('',(#5519,#5520,#5521));
#1480=EDGE_LOOP('',(#5522,#5523,#5524,#5525));
#1481=EDGE_LOOP('',(#5526,#5527,#5528,#5529));
#1482=EDGE_LOOP('',(#5530,#5531,#5532));
#1483=EDGE_LOOP('',(#5533,#5534,#5535,#5536));
#1484=EDGE_LOOP('',(#5537,#5538,#5539,#5540));
#1485=EDGE_LOOP('',(#5541,#5542,#5543,#5544));
#1486=EDGE_LOOP('',(#5545,#5546,#5547,#5548));
#1487=EDGE_LOOP('',(#5549,#5550,#5551,#5552));
#1488=EDGE_LOOP('',(#5553,#5554,#5555,#5556));
#1489=EDGE_LOOP('',(#5557,#5558,#5559,#5560));
#1490=EDGE_LOOP('',(#5561,#5562,#5563,#5564,#5565,#5566,#5567,#5568));
#1491=EDGE_LOOP('',(#5569,#5570,#5571,#5572));
#1492=EDGE_LOOP('',(#5573,#5574,#5575,#5576,#5577,#5578));
#1493=EDGE_LOOP('',(#5579,#5580,#5581,#5582,#5583,#5584));
#1494=EDGE_LOOP('',(#5585));
#1495=EDGE_LOOP('',(#5586));
#1496=EDGE_LOOP('',(#5587));
#1497=EDGE_LOOP('',(#5588));
#1498=EDGE_LOOP('',(#5589,#5590,#5591,#5592));
#1499=EDGE_LOOP('',(#5593,#5594,#5595,#5596));
#1500=EDGE_LOOP('',(#5597,#5598,#5599,#5600));
#1501=EDGE_LOOP('',(#5601,#5602,#5603,#5604));
#1502=EDGE_LOOP('',(#5605));
#1503=EDGE_LOOP('',(#5606));
#1504=EDGE_LOOP('',(#5607,#5608,#5609,#5610));
#1505=EDGE_LOOP('',(#5611));
#1506=EDGE_LOOP('',(#5612));
#1507=EDGE_LOOP('',(#5613));
#1508=EDGE_LOOP('',(#5614,#5615,#5616,#5617));
#1509=EDGE_LOOP('',(#5618));
#1510=EDGE_LOOP('',(#5619));
#1511=EDGE_LOOP('',(#5620));
#1512=EDGE_LOOP('',(#5621,#5622,#5623,#5624));
#1513=EDGE_LOOP('',(#5625));
#1514=EDGE_LOOP('',(#5626));
#1515=EDGE_LOOP('',(#5627));
#1516=EDGE_LOOP('',(#5628,#5629,#5630,#5631));
#1517=EDGE_LOOP('',(#5632));
#1518=EDGE_LOOP('',(#5633,#5634,#5635,#5636));
#1519=EDGE_LOOP('',(#5637,#5638,#5639,#5640));
#1520=EDGE_LOOP('',(#5641,#5642,#5643,#5644));
#1521=EDGE_LOOP('',(#5645,#5646,#5647,#5648));
#1522=EDGE_LOOP('',(#5649,#5650,#5651,#5652));
#1523=EDGE_LOOP('',(#5653,#5654,#5655,#5656));
#1524=EDGE_LOOP('',(#5657,#5658,#5659,#5660));
#1525=EDGE_LOOP('',(#5661,#5662,#5663,#5664));
#1526=EDGE_LOOP('',(#5665,#5666,#5667,#5668));
#1527=EDGE_LOOP('',(#5669,#5670,#5671,#5672));
#1528=EDGE_LOOP('',(#5673,#5674,#5675,#5676));
#1529=EDGE_LOOP('',(#5677,#5678,#5679,#5680));
#1530=EDGE_LOOP('',(#5681,#5682,#5683,#5684));
#1531=EDGE_LOOP('',(#5685,#5686,#5687,#5688));
#1532=EDGE_LOOP('',(#5689,#5690,#5691,#5692));
#1533=EDGE_LOOP('',(#5693,#5694,#5695,#5696));
#1534=EDGE_LOOP('',(#5697,#5698,#5699,#5700,#5701,#5702,#5703,#5704));
#1535=EDGE_LOOP('',(#5705));
#1536=EDGE_LOOP('',(#5706));
#1537=EDGE_LOOP('',(#5707,#5708,#5709,#5710));
#1538=EDGE_LOOP('',(#5711,#5712,#5713,#5714));
#1539=EDGE_LOOP('',(#5715,#5716,#5717,#5718));
#1540=EDGE_LOOP('',(#5719,#5720,#5721,#5722,#5723,#5724,#5725,#5726));
#1541=EDGE_LOOP('',(#5727));
#1542=EDGE_LOOP('',(#5728));
#1543=EDGE_LOOP('',(#5729));
#1544=EDGE_LOOP('',(#5730));
#1545=EDGE_LOOP('',(#5731));
#1546=EDGE_LOOP('',(#5732));
#1547=EDGE_LOOP('',(#5733,#5734,#5735,#5736));
#1548=EDGE_LOOP('',(#5737,#5738,#5739,#5740));
#1549=EDGE_LOOP('',(#5741,#5742,#5743,#5744));
#1550=EDGE_LOOP('',(#5745,#5746,#5747,#5748));
#1551=EDGE_LOOP('',(#5749,#5750,#5751,#5752));
#1552=EDGE_LOOP('',(#5753,#5754,#5755,#5756));
#1553=EDGE_LOOP('',(#5757,#5758,#5759,#5760));
#1554=EDGE_LOOP('',(#5761,#5762,#5763,#5764));
#1555=EDGE_LOOP('',(#5765,#5766,#5767,#5768));
#1556=EDGE_LOOP('',(#5769,#5770,#5771,#5772));
#1557=EDGE_LOOP('',(#5773,#5774,#5775,#5776));
#1558=EDGE_LOOP('',(#5777,#5778,#5779,#5780));
#1559=EDGE_LOOP('',(#5781,#5782,#5783,#5784));
#1560=EDGE_LOOP('',(#5785,#5786,#5787,#5788));
#1561=EDGE_LOOP('',(#5789,#5790,#5791,#5792));
#1562=EDGE_LOOP('',(#5793,#5794,#5795,#5796));
#1563=EDGE_LOOP('',(#5797,#5798,#5799,#5800));
#1564=EDGE_LOOP('',(#5801,#5802,#5803,#5804));
#1565=EDGE_LOOP('',(#5805,#5806,#5807,#5808));
#1566=EDGE_LOOP('',(#5809,#5810,#5811,#5812));
#1567=EDGE_LOOP('',(#5813,#5814,#5815,#5816));
#1568=EDGE_LOOP('',(#5817,#5818,#5819,#5820));
#1569=EDGE_LOOP('',(#5821,#5822,#5823,#5824));
#1570=EDGE_LOOP('',(#5825,#5826,#5827,#5828));
#1571=EDGE_LOOP('',(#5829,#5830,#5831,#5832));
#1572=EDGE_LOOP('',(#5833,#5834,#5835,#5836));
#1573=EDGE_LOOP('',(#5837,#5838,#5839,#5840));
#1574=EDGE_LOOP('',(#5841,#5842,#5843,#5844));
#1575=EDGE_LOOP('',(#5845,#5846,#5847,#5848));
#1576=EDGE_LOOP('',(#5849,#5850,#5851,#5852));
#1577=EDGE_LOOP('',(#5853,#5854,#5855,#5856));
#1578=EDGE_LOOP('',(#5857,#5858,#5859,#5860));
#1579=EDGE_LOOP('',(#5861,#5862,#5863,#5864));
#1580=EDGE_LOOP('',(#5865,#5866,#5867,#5868));
#1581=EDGE_LOOP('',(#5869,#5870,#5871,#5872));
#1582=EDGE_LOOP('',(#5873,#5874,#5875,#5876));
#1583=EDGE_LOOP('',(#5877,#5878,#5879,#5880));
#1584=EDGE_LOOP('',(#5881,#5882,#5883,#5884));
#1585=EDGE_LOOP('',(#5885,#5886,#5887,#5888));
#1586=EDGE_LOOP('',(#5889,#5890,#5891,#5892));
#1587=EDGE_LOOP('',(#5893,#5894,#5895,#5896));
#1588=EDGE_LOOP('',(#5897,#5898,#5899,#5900));
#1589=EDGE_LOOP('',(#5901,#5902,#5903,#5904));
#1590=EDGE_LOOP('',(#5905,#5906,#5907,#5908));
#1591=EDGE_LOOP('',(#5909,#5910,#5911,#5912));
#1592=EDGE_LOOP('',(#5913,#5914,#5915,#5916));
#1593=EDGE_LOOP('',(#5917,#5918,#5919,#5920));
#1594=EDGE_LOOP('',(#5921,#5922,#5923,#5924));
#1595=EDGE_LOOP('',(#5925,#5926,#5927,#5928));
#1596=EDGE_LOOP('',(#5929,#5930,#5931,#5932));
#1597=EDGE_LOOP('',(#5933,#5934,#5935,#5936));
#1598=EDGE_LOOP('',(#5937,#5938,#5939,#5940));
#1599=EDGE_LOOP('',(#5941,#5942,#5943,#5944));
#1600=EDGE_LOOP('',(#5945,#5946,#5947,#5948));
#1601=EDGE_LOOP('',(#5949,#5950,#5951,#5952));
#1602=EDGE_LOOP('',(#5953,#5954,#5955,#5956));
#1603=EDGE_LOOP('',(#5957,#5958,#5959,#5960));
#1604=EDGE_LOOP('',(#5961,#5962,#5963,#5964));
#1605=EDGE_LOOP('',(#5965,#5966,#5967,#5968));
#1606=EDGE_LOOP('',(#5969,#5970,#5971,#5972));
#1607=EDGE_LOOP('',(#5973,#5974,#5975,#5976));
#1608=EDGE_LOOP('',(#5977,#5978,#5979,#5980,#5981,#5982,#5983,#5984));
#1609=EDGE_LOOP('',(#5985,#5986,#5987,#5988,#5989,#5990,#5991,#5992,#5993,
#5994,#5995,#5996,#5997,#5998,#5999,#6000,#6001,#6002,#6003,#6004,#6005,
#6006,#6007,#6008,#6009,#6010,#6011,#6012,#6013,#6014,#6015,#6016,#6017,
#6018,#6019,#6020,#6021,#6022,#6023,#6024,#6025,#6026,#6027,#6028,#6029,
#6030,#6031,#6032,#6033,#6034,#6035,#6036,#6037,#6038,#6039,#6040,#6041,
#6042,#6043,#6044,#6045,#6046,#6047,#6048));
#1610=EDGE_LOOP('',(#6049,#6050,#6051,#6052));
#1611=EDGE_LOOP('',(#6053,#6054,#6055,#6056,#6057,#6058,#6059,#6060,#6061,
#6062,#6063,#6064,#6065,#6066,#6067,#6068,#6069,#6070,#6071,#6072,#6073,
#6074,#6075,#6076,#6077,#6078,#6079,#6080,#6081,#6082,#6083,#6084,#6085,
#6086,#6087,#6088,#6089,#6090,#6091,#6092,#6093,#6094,#6095,#6096,#6097,
#6098,#6099,#6100,#6101,#6102,#6103,#6104,#6105,#6106,#6107,#6108,#6109,
#6110,#6111,#6112,#6113,#6114,#6115,#6116,#6117));
#1612=EDGE_LOOP('',(#6118,#6119,#6120,#6121));
#1613=EDGE_LOOP('',(#6122,#6123,#6124,#6125));
#1614=EDGE_LOOP('',(#6126,#6127,#6128,#6129));
#1615=EDGE_LOOP('',(#6130,#6131,#6132,#6133));
#1616=EDGE_LOOP('',(#6134,#6135,#6136,#6137));
#1617=EDGE_LOOP('',(#6138,#6139,#6140,#6141));
#1618=EDGE_LOOP('',(#6142,#6143,#6144,#6145));
#1619=EDGE_LOOP('',(#6146,#6147,#6148,#6149,#6150,#6151));
#1620=EDGE_LOOP('',(#6152));
#1621=EDGE_LOOP('',(#6153,#6154,#6155,#6156));
#1622=EDGE_LOOP('',(#6157,#6158,#6159,#6160));
#1623=EDGE_LOOP('',(#6161));
#1624=EDGE_LOOP('',(#6162,#6163,#6164,#6165,#6166,#6167));
#1625=EDGE_LOOP('',(#6168));
#1626=EDGE_LOOP('',(#6169,#6170,#6171));
#1627=EDGE_LOOP('',(#6172,#6173,#6174,#6175,#6176));
#1628=EDGE_LOOP('',(#6177,#6178,#6179,#6180));
#1629=EDGE_LOOP('',(#6181,#6182,#6183,#6184));
#1630=EDGE_LOOP('',(#6185,#6186,#6187,#6188));
#1631=EDGE_LOOP('',(#6189,#6190,#6191,#6192));
#1632=EDGE_LOOP('',(#6193,#6194,#6195,#6196));
#1633=EDGE_LOOP('',(#6197,#6198,#6199,#6200));
#1634=EDGE_LOOP('',(#6201,#6202,#6203,#6204));
#1635=EDGE_LOOP('',(#6205,#6206,#6207,#6208));
#1636=EDGE_LOOP('',(#6209,#6210,#6211,#6212));
#1637=EDGE_LOOP('',(#6213,#6214,#6215,#6216,#6217,#6218,#6219,#6220,#6221,
#6222,#6223,#6224,#6225,#6226));
#1638=EDGE_LOOP('',(#6227,#6228,#6229,#6230,#6231,#6232,#6233,#6234,#6235,
#6236,#6237,#6238,#6239));
#1639=EDGE_LOOP('',(#6240,#6241,#6242,#6243,#6244,#6245));
#1640=EDGE_LOOP('',(#6246,#6247,#6248,#6249));
#1641=EDGE_LOOP('',(#6250,#6251,#6252,#6253));
#1642=EDGE_LOOP('',(#6254,#6255,#6256,#6257));
#1643=EDGE_LOOP('',(#6258,#6259,#6260,#6261));
#1644=EDGE_LOOP('',(#6262,#6263,#6264,#6265));
#1645=EDGE_LOOP('',(#6266,#6267,#6268,#6269));
#1646=EDGE_LOOP('',(#6270,#6271,#6272,#6273));
#1647=EDGE_LOOP('',(#6274,#6275,#6276,#6277));
#1648=EDGE_LOOP('',(#6278,#6279,#6280,#6281,#6282,#6283));
#1649=EDGE_LOOP('',(#6284,#6285,#6286,#6287,#6288));
#1650=EDGE_LOOP('',(#6289,#6290,#6291,#6292));
#1651=EDGE_LOOP('',(#6293,#6294,#6295,#6296));
#1652=EDGE_LOOP('',(#6297));
#1653=EDGE_LOOP('',(#6298));
#1654=EDGE_LOOP('',(#6299));
#1655=EDGE_LOOP('',(#6300));
#1656=LINE('',#8884,#2105);
#1657=LINE('',#8890,#2106);
#1658=LINE('',#8896,#2107);
#1659=LINE('',#8901,#2108);
#1660=LINE('',#8903,#2109);
#1661=LINE('',#8904,#2110);
#1662=LINE('',#8908,#2111);
#1663=LINE('',#8909,#2112);
#1664=LINE('',#8910,#2113);
#1665=LINE('',#8913,#2114);
#1666=LINE('',#8914,#2115);
#1667=LINE('',#8917,#2116);
#1668=LINE('',#8919,#2117);
#1669=LINE('',#8921,#2118);
#1670=LINE('',#8923,#2119);
#1671=LINE('',#8925,#2120);
#1672=LINE('',#8926,#2121);
#1673=LINE('',#8929,#2122);
#1674=LINE('',#8930,#2123);
#1675=LINE('',#8933,#2124);
#1676=LINE('',#8934,#2125);
#1677=LINE('',#8937,#2126);
#1678=LINE('',#8938,#2127);
#1679=LINE('',#8943,#2128);
#1680=LINE('',#8945,#2129);
#1681=LINE('',#8947,#2130);
#1682=LINE('',#8949,#2131);
#1683=LINE('',#8951,#2132);
#1684=LINE('',#8953,#2133);
#1685=LINE('',#8957,#2134);
#1686=LINE('',#8959,#2135);
#1687=LINE('',#8961,#2136);
#1688=LINE('',#8963,#2137);
#1689=LINE('',#8964,#2138);
#1690=LINE('',#8967,#2139);
#1691=LINE('',#8969,#2140);
#1692=LINE('',#8970,#2141);
#1693=LINE('',#8973,#2142);
#1694=LINE('',#8975,#2143);
#1695=LINE('',#8977,#2144);
#1696=LINE('',#8978,#2145);
#1697=LINE('',#8980,#2146);
#1698=LINE('',#8983,#2147);
#1699=LINE('',#8985,#2148);
#1700=LINE('',#8986,#2149);
#1701=LINE('',#8988,#2150);
#1702=LINE('',#8990,#2151);
#1703=LINE('',#8992,#2152);
#1704=LINE('',#8997,#2153);
#1705=LINE('',#8999,#2154);
#1706=LINE('',#9001,#2155);
#1707=LINE('',#9003,#2156);
#1708=LINE('',#9005,#2157);
#1709=LINE('',#9007,#2158);
#1710=LINE('',#9010,#2159);
#1711=LINE('',#9012,#2160);
#1712=LINE('',#9013,#2161);
#1713=LINE('',#9015,#2162);
#1714=LINE('',#9017,#2163);
#1715=LINE('',#9019,#2164);
#1716=LINE('',#9021,#2165);
#1717=LINE('',#9029,#2166);
#1718=LINE('',#9035,#2167);
#1719=LINE('',#9041,#2168);
#1720=LINE('',#9046,#2169);
#1721=LINE('',#9048,#2170);
#1722=LINE('',#9050,#2171);
#1723=LINE('',#9051,#2172);
#1724=LINE('',#9054,#2173);
#1725=LINE('',#9056,#2174);
#1726=LINE('',#9058,#2175);
#1727=LINE('',#9059,#2176);
#1728=LINE('',#9063,#2177);
#1729=LINE('',#9065,#2178);
#1730=LINE('',#9066,#2179);
#1731=LINE('',#9067,#2180);
#1732=LINE('',#9071,#2181);
#1733=LINE('',#9073,#2182);
#1734=LINE('',#9075,#2183);
#1735=LINE('',#9076,#2184);
#1736=LINE('',#9079,#2185);
#1737=LINE('',#9080,#2186);
#1738=LINE('',#9083,#2187);
#1739=LINE('',#9084,#2188);
#1740=LINE('',#9086,#2189);
#1741=LINE('',#9087,#2190);
#1742=LINE('',#9092,#2191);
#1743=LINE('',#9094,#2192);
#1744=LINE('',#9096,#2193);
#1745=LINE('',#9098,#2194);
#1746=LINE('',#9100,#2195);
#1747=LINE('',#9102,#2196);
#1748=LINE('',#9107,#2197);
#1749=LINE('',#9110,#2198);
#1750=LINE('',#9112,#2199);
#1751=LINE('',#9113,#2200);
#1752=LINE('',#9116,#2201);
#1753=LINE('',#9117,#2202);
#1754=LINE('',#9120,#2203);
#1755=LINE('',#9121,#2204);
#1756=LINE('',#9124,#2205);
#1757=LINE('',#9125,#2206);
#1758=LINE('',#9128,#2207);
#1759=LINE('',#9129,#2208);
#1760=LINE('',#9131,#2209);
#1761=LINE('',#9140,#2210);
#1762=LINE('',#9151,#2211);
#1763=LINE('',#9159,#2212);
#1764=LINE('',#9163,#2213);
#1765=LINE('',#9169,#2214);
#1766=LINE('',#9171,#2215);
#1767=LINE('',#9173,#2216);
#1768=LINE('',#9174,#2217);
#1769=LINE('',#9178,#2218);
#1770=LINE('',#9180,#2219);
#1771=LINE('',#9182,#2220);
#1772=LINE('',#9183,#2221);
#1773=LINE('',#9202,#2222);
#1774=LINE('',#9234,#2223);
#1775=LINE('',#9269,#2224);
#1776=LINE('',#9274,#2225);
#1777=LINE('',#9278,#2226);
#1778=LINE('',#9283,#2227);
#1779=LINE('',#9289,#2228);
#1780=LINE('',#9298,#2229);
#1781=LINE('',#9305,#2230);
#1782=LINE('',#9309,#2231);
#1783=LINE('',#9314,#2232);
#1784=LINE('',#9316,#2233);
#1785=LINE('',#9318,#2234);
#1786=LINE('',#9319,#2235);
#1787=LINE('',#9323,#2236);
#1788=LINE('',#9325,#2237);
#1789=LINE('',#9327,#2238);
#1790=LINE('',#9328,#2239);
#1791=LINE('',#9332,#2240);
#1792=LINE('',#9334,#2241);
#1793=LINE('',#9336,#2242);
#1794=LINE('',#9337,#2243);
#1795=LINE('',#9341,#2244);
#1796=LINE('',#9343,#2245);
#1797=LINE('',#9345,#2246);
#1798=LINE('',#9346,#2247);
#1799=LINE('',#9350,#2248);
#1800=LINE('',#9352,#2249);
#1801=LINE('',#9354,#2250);
#1802=LINE('',#9355,#2251);
#1803=LINE('',#9359,#2252);
#1804=LINE('',#9361,#2253);
#1805=LINE('',#9363,#2254);
#1806=LINE('',#9364,#2255);
#1807=LINE('',#9368,#2256);
#1808=LINE('',#9370,#2257);
#1809=LINE('',#9372,#2258);
#1810=LINE('',#9373,#2259);
#1811=LINE('',#9381,#2260);
#1812=LINE('',#9382,#2261);
#1813=LINE('',#9384,#2262);
#1814=LINE('',#9385,#2263);
#1815=LINE('',#9387,#2264);
#1816=LINE('',#9388,#2265);
#1817=LINE('',#9391,#2266);
#1818=LINE('',#9393,#2267);
#1819=LINE('',#9394,#2268);
#1820=LINE('',#9397,#2269);
#1821=LINE('',#9399,#2270);
#1822=LINE('',#9400,#2271);
#1823=LINE('',#9404,#2272);
#1824=LINE('',#9442,#2273);
#1825=LINE('',#9480,#2274);
#1826=LINE('',#9518,#2275);
#1827=LINE('',#9555,#2276);
#1828=LINE('',#9558,#2277);
#1829=LINE('',#9596,#2278);
#1830=LINE('',#9633,#2279);
#1831=LINE('',#9636,#2280);
#1832=LINE('',#9708,#2281);
#1833=LINE('',#9711,#2282);
#1834=LINE('',#9718,#2283);
#1835=LINE('',#9724,#2284);
#1836=LINE('',#9735,#2285);
#1837=LINE('',#9747,#2286);
#1838=LINE('',#9753,#2287);
#1839=LINE('',#9788,#2288);
#1840=LINE('',#9877,#2289);
#1841=LINE('',#9965,#2290);
#1842=LINE('',#10000,#2291);
#1843=LINE('',#10006,#2292);
#1844=LINE('',#10018,#2293);
#1845=LINE('',#10061,#2294);
#1846=LINE('',#10102,#2295);
#1847=LINE('',#10106,#2296);
#1848=LINE('',#10108,#2297);
#1849=LINE('',#10154,#2298);
#1850=LINE('',#10289,#2299);
#1851=LINE('',#10393,#2300);
#1852=LINE('',#10707,#2301);
#1853=LINE('',#10796,#2302);
#1854=LINE('',#10884,#2303);
#1855=LINE('',#11004,#2304);
#1856=LINE('',#11005,#2305);
#1857=LINE('',#11042,#2306);
#1858=LINE('',#11043,#2307);
#1859=LINE('',#11250,#2308);
#1860=LINE('',#11282,#2309);
#1861=LINE('',#11317,#2310);
#1862=LINE('',#11322,#2311);
#1863=LINE('',#11326,#2312);
#1864=LINE('',#11331,#2313);
#1865=LINE('',#11336,#2314);
#1866=LINE('',#11338,#2315);
#1867=LINE('',#11340,#2316);
#1868=LINE('',#11341,#2317);
#1869=LINE('',#11344,#2318);
#1870=LINE('',#11346,#2319);
#1871=LINE('',#11347,#2320);
#1872=LINE('',#11350,#2321);
#1873=LINE('',#11352,#2322);
#1874=LINE('',#11353,#2323);
#1875=LINE('',#11356,#2324);
#1876=LINE('',#11358,#2325);
#1877=LINE('',#11359,#2326);
#1878=LINE('',#11362,#2327);
#1879=LINE('',#11364,#2328);
#1880=LINE('',#11365,#2329);
#1881=LINE('',#11367,#2330);
#1882=LINE('',#11368,#2331);
#1883=LINE('',#11375,#2332);
#1884=LINE('',#11377,#2333);
#1885=LINE('',#11379,#2334);
#1886=LINE('',#11380,#2335);
#1887=LINE('',#11383,#2336);
#1888=LINE('',#11385,#2337);
#1889=LINE('',#11386,#2338);
#1890=LINE('',#11389,#2339);
#1891=LINE('',#11391,#2340);
#1892=LINE('',#11392,#2341);
#1893=LINE('',#11395,#2342);
#1894=LINE('',#11397,#2343);
#1895=LINE('',#11398,#2344);
#1896=LINE('',#11401,#2345);
#1897=LINE('',#11403,#2346);
#1898=LINE('',#11404,#2347);
#1899=LINE('',#11406,#2348);
#1900=LINE('',#11407,#2349);
#1901=LINE('',#11413,#2350);
#1902=LINE('',#11417,#2351);
#1903=LINE('',#11422,#2352);
#1904=LINE('',#11424,#2353);
#1905=LINE('',#11426,#2354);
#1906=LINE('',#11427,#2355);
#1907=LINE('',#11431,#2356);
#1908=LINE('',#11433,#2357);
#1909=LINE('',#11435,#2358);
#1910=LINE('',#11436,#2359);
#1911=LINE('',#11440,#2360);
#1912=LINE('',#11442,#2361);
#1913=LINE('',#11444,#2362);
#1914=LINE('',#11445,#2363);
#1915=LINE('',#11449,#2364);
#1916=LINE('',#11451,#2365);
#1917=LINE('',#11453,#2366);
#1918=LINE('',#11454,#2367);
#1919=LINE('',#11458,#2368);
#1920=LINE('',#11460,#2369);
#1921=LINE('',#11462,#2370);
#1922=LINE('',#11463,#2371);
#1923=LINE('',#11467,#2372);
#1924=LINE('',#11469,#2373);
#1925=LINE('',#11471,#2374);
#1926=LINE('',#11472,#2375);
#1927=LINE('',#11476,#2376);
#1928=LINE('',#11478,#2377);
#1929=LINE('',#11480,#2378);
#1930=LINE('',#11481,#2379);
#1931=LINE('',#11489,#2380);
#1932=LINE('',#11490,#2381);
#1933=LINE('',#11492,#2382);
#1934=LINE('',#11493,#2383);
#1935=LINE('',#11495,#2384);
#1936=LINE('',#11496,#2385);
#1937=LINE('',#11499,#2386);
#1938=LINE('',#11501,#2387);
#1939=LINE('',#11502,#2388);
#1940=LINE('',#11505,#2389);
#1941=LINE('',#11507,#2390);
#1942=LINE('',#11508,#2391);
#1943=LINE('',#11512,#2392);
#1944=LINE('',#11550,#2393);
#1945=LINE('',#11588,#2394);
#1946=LINE('',#11626,#2395);
#1947=LINE('',#11663,#2396);
#1948=LINE('',#11666,#2397);
#1949=LINE('',#11704,#2398);
#1950=LINE('',#11741,#2399);
#1951=LINE('',#11744,#2400);
#1952=LINE('',#11816,#2401);
#1953=LINE('',#11819,#2402);
#1954=LINE('',#11826,#2403);
#1955=LINE('',#11832,#2404);
#1956=LINE('',#11843,#2405);
#1957=LINE('',#11855,#2406);
#1958=LINE('',#11861,#2407);
#1959=LINE('',#11896,#2408);
#1960=LINE('',#11985,#2409);
#1961=LINE('',#12073,#2410);
#1962=LINE('',#12108,#2411);
#1963=LINE('',#12114,#2412);
#1964=LINE('',#12126,#2413);
#1965=LINE('',#12169,#2414);
#1966=LINE('',#12210,#2415);
#1967=LINE('',#12214,#2416);
#1968=LINE('',#12216,#2417);
#1969=LINE('',#12262,#2418);
#1970=LINE('',#12397,#2419);
#1971=LINE('',#12501,#2420);
#1972=LINE('',#12815,#2421);
#1973=LINE('',#12904,#2422);
#1974=LINE('',#12992,#2423);
#1975=LINE('',#13112,#2424);
#1976=LINE('',#13113,#2425);
#1977=LINE('',#13150,#2426);
#1978=LINE('',#13151,#2427);
#1979=LINE('',#13354,#2428);
#1980=LINE('',#13360,#2429);
#1981=LINE('',#13370,#2430);
#1982=LINE('',#13380,#2431);
#1983=LINE('',#13390,#2432);
#1984=LINE('',#13400,#2433);
#1985=LINE('',#13404,#2434);
#1986=LINE('',#13408,#2435);
#1987=LINE('',#13412,#2436);
#1988=LINE('',#13416,#2437);
#1989=LINE('',#13463,#2438);
#1990=LINE('',#13464,#2439);
#1991=LINE('',#13583,#2440);
#1992=LINE('',#13584,#2441);
#1993=LINE('',#13665,#2442);
#1994=LINE('',#13818,#2443);
#1995=LINE('',#13960,#2444);
#1996=LINE('',#13984,#2445);
#1997=LINE('',#14032,#2446);
#1998=LINE('',#14080,#2447);
#1999=LINE('',#14131,#2448);
#2000=LINE('',#14179,#2449);
#2001=LINE('',#14227,#2450);
#2002=LINE('',#14275,#2451);
#2003=LINE('',#14329,#2452);
#2004=LINE('',#14377,#2453);
#2005=LINE('',#14425,#2454);
#2006=LINE('',#14479,#2455);
#2007=LINE('',#14527,#2456);
#2008=LINE('',#14575,#2457);
#2009=LINE('',#14623,#2458);
#2010=LINE('',#14677,#2459);
#2011=LINE('',#14725,#2460);
#2012=LINE('',#14773,#2461);
#2013=LINE('',#14827,#2462);
#2014=LINE('',#14875,#2463);
#2015=LINE('',#14923,#2464);
#2016=LINE('',#14977,#2465);
#2017=LINE('',#15025,#2466);
#2018=LINE('',#15073,#2467);
#2019=LINE('',#15121,#2468);
#2020=LINE('',#15175,#2469);
#2021=LINE('',#15223,#2470);
#2022=LINE('',#15271,#2471);
#2023=LINE('',#15325,#2472);
#2024=LINE('',#15373,#2473);
#2025=LINE('',#15421,#2474);
#2026=LINE('',#15447,#2475);
#2027=LINE('',#15471,#2476);
#2028=LINE('',#15495,#2477);
#2029=LINE('',#15520,#2478);
#2030=LINE('',#15545,#2479);
#2031=LINE('',#15569,#2480);
#2032=LINE('',#15594,#2481);
#2033=LINE('',#15619,#2482);
#2034=LINE('',#15643,#2483);
#2035=LINE('',#15667,#2484);
#2036=LINE('',#15692,#2485);
#2037=LINE('',#15717,#2486);
#2038=LINE('',#15741,#2487);
#2039=LINE('',#15766,#2488);
#2040=LINE('',#15791,#2489);
#2041=LINE('',#15815,#2490);
#2042=LINE('',#15840,#2491);
#2043=LINE('',#15865,#2492);
#2044=LINE('',#15889,#2493);
#2045=LINE('',#15913,#2494);
#2046=LINE('',#15938,#2495);
#2047=LINE('',#15963,#2496);
#2048=LINE('',#15987,#2497);
#2049=LINE('',#16012,#2498);
#2050=LINE('',#16037,#2499);
#2051=LINE('',#16061,#2500);
#2052=LINE('',#16086,#2501);
#2053=LINE('',#16110,#2502);
#2054=LINE('',#16135,#2503);
#2055=LINE('',#16336,#2504);
#2056=LINE('',#18081,#2505);
#2057=LINE('',#18083,#2506);
#2058=LINE('',#18085,#2507);
#2059=LINE('',#18086,#2508);
#2060=LINE('',#18089,#2509);
#2061=LINE('',#18091,#2510);
#2062=LINE('',#18092,#2511);
#2063=LINE('',#18095,#2512);
#2064=LINE('',#18097,#2513);
#2065=LINE('',#18098,#2514);
#2066=LINE('',#18101,#2515);
#2067=LINE('',#18103,#2516);
#2068=LINE('',#18104,#2517);
#2069=LINE('',#18107,#2518);
#2070=LINE('',#18109,#2519);
#2071=LINE('',#18110,#2520);
#2072=LINE('',#18112,#2521);
#2073=LINE('',#18113,#2522);
#2074=LINE('',#18120,#2523);
#2075=LINE('',#18128,#2524);
#2076=LINE('',#18141,#2525);
#2077=LINE('',#18188,#2526);
#2078=LINE('',#18242,#2527);
#2079=LINE('',#18290,#2528);
#2080=LINE('',#18329,#2529);
#2081=LINE('',#18350,#2530);
#2082=LINE('',#18375,#2531);
#2083=LINE('',#18400,#2532);
#2084=LINE('',#18425,#2533);
#2085=LINE('',#18998,#2534);
#2086=LINE('',#19000,#2535);
#2087=LINE('',#19002,#2536);
#2088=LINE('',#19004,#2537);
#2089=LINE('',#19006,#2538);
#2090=LINE('',#19007,#2539);
#2091=LINE('',#19012,#2540);
#2092=LINE('',#19013,#2541);
#2093=LINE('',#19014,#2542);
#2094=LINE('',#19017,#2543);
#2095=LINE('',#19018,#2544);
#2096=LINE('',#19021,#2545);
#2097=LINE('',#19022,#2546);
#2098=LINE('',#19025,#2547);
#2099=LINE('',#19026,#2548);
#2100=LINE('',#19029,#2549);
#2101=LINE('',#19030,#2550);
#2102=LINE('',#19032,#2551);
#2103=LINE('',#19047,#2552);
#2104=LINE('',#19053,#2553);
#2105=VECTOR('',#7445,0.17);
#2106=VECTOR('',#7452,0.17);
#2107=VECTOR('',#7459,0.41);
#2108=VECTOR('',#7464,1.);
#2109=VECTOR('',#7465,1.);
#2110=VECTOR('',#7466,1.);
#2111=VECTOR('',#7469,1.);
#2112=VECTOR('',#7470,1.);
#2113=VECTOR('',#7471,1.);
#2114=VECTOR('',#7474,1.);
#2115=VECTOR('',#7475,1.);
#2116=VECTOR('',#7478,1.);
#2117=VECTOR('',#7479,1.);
#2118=VECTOR('',#7480,1.);
#2119=VECTOR('',#7481,1.);
#2120=VECTOR('',#7482,1.);
#2121=VECTOR('',#7483,1.);
#2122=VECTOR('',#7486,1.);
#2123=VECTOR('',#7487,1.);
#2124=VECTOR('',#7490,1.);
#2125=VECTOR('',#7491,1.);
#2126=VECTOR('',#7494,1.);
#2127=VECTOR('',#7495,1.);
#2128=VECTOR('',#7500,1.);
#2129=VECTOR('',#7501,1.);
#2130=VECTOR('',#7502,1.);
#2131=VECTOR('',#7503,1.);
#2132=VECTOR('',#7504,1.);
#2133=VECTOR('',#7505,1.);
#2134=VECTOR('',#7508,1.);
#2135=VECTOR('',#7509,1.);
#2136=VECTOR('',#7510,1.);
#2137=VECTOR('',#7511,1.);
#2138=VECTOR('',#7512,1.);
#2139=VECTOR('',#7515,1.);
#2140=VECTOR('',#7516,1.);
#2141=VECTOR('',#7517,1.);
#2142=VECTOR('',#7520,1.);
#2143=VECTOR('',#7521,1.);
#2144=VECTOR('',#7522,1.);
#2145=VECTOR('',#7523,1.);
#2146=VECTOR('',#7526,1.);
#2147=VECTOR('',#7529,1.);
#2148=VECTOR('',#7530,1.);
#2149=VECTOR('',#7531,1.);
#2150=VECTOR('',#7534,1.);
#2151=VECTOR('',#7537,1.);
#2152=VECTOR('',#7540,1.);
#2153=VECTOR('',#7545,1.);
#2154=VECTOR('',#7546,1.);
#2155=VECTOR('',#7547,1.);
#2156=VECTOR('',#7548,1.);
#2157=VECTOR('',#7549,1.);
#2158=VECTOR('',#7550,1.);
#2159=VECTOR('',#7555,1.);
#2160=VECTOR('',#7558,1.);
#2161=VECTOR('',#7559,1.);
#2162=VECTOR('',#7562,1.);
#2163=VECTOR('',#7565,1.);
#2164=VECTOR('',#7568,1.);
#2165=VECTOR('',#7571,1.);
#2166=VECTOR('',#7582,0.17);
#2167=VECTOR('',#7589,0.17);
#2168=VECTOR('',#7596,0.41);
#2169=VECTOR('',#7601,1.);
#2170=VECTOR('',#7602,1.);
#2171=VECTOR('',#7603,1.);
#2172=VECTOR('',#7604,1.);
#2173=VECTOR('',#7607,1.);
#2174=VECTOR('',#7608,1.);
#2175=VECTOR('',#7609,1.);
#2176=VECTOR('',#7610,1.);
#2177=VECTOR('',#7613,1.);
#2178=VECTOR('',#7614,1.);
#2179=VECTOR('',#7615,1.);
#2180=VECTOR('',#7616,1.);
#2181=VECTOR('',#7619,1.);
#2182=VECTOR('',#7620,1.);
#2183=VECTOR('',#7621,1.);
#2184=VECTOR('',#7622,1.);
#2185=VECTOR('',#7625,1.);
#2186=VECTOR('',#7626,1.);
#2187=VECTOR('',#7629,1.);
#2188=VECTOR('',#7630,1.);
#2189=VECTOR('',#7633,1.);
#2190=VECTOR('',#7634,1.);
#2191=VECTOR('',#7639,1.);
#2192=VECTOR('',#7640,1.);
#2193=VECTOR('',#7641,1.);
#2194=VECTOR('',#7642,1.);
#2195=VECTOR('',#7643,1.);
#2196=VECTOR('',#7644,1.);
#2197=VECTOR('',#7651,1.);
#2198=VECTOR('',#7654,1.);
#2199=VECTOR('',#7655,1.);
#2200=VECTOR('',#7656,1.);
#2201=VECTOR('',#7659,1.);
#2202=VECTOR('',#7660,1.);
#2203=VECTOR('',#7663,1.);
#2204=VECTOR('',#7664,1.);
#2205=VECTOR('',#7667,1.);
#2206=VECTOR('',#7668,1.);
#2207=VECTOR('',#7671,1.);
#2208=VECTOR('',#7672,1.);
#2209=VECTOR('',#7675,1.);
#2210=VECTOR('',#7688,0.3);
#2211=VECTOR('',#7703,0.4);
#2212=VECTOR('',#7712,0.6);
#2213=VECTOR('',#7719,0.4);
#2214=VECTOR('',#7726,1.);
#2215=VECTOR('',#7727,1.);
#2216=VECTOR('',#7728,1.);
#2217=VECTOR('',#7729,1.);
#2218=VECTOR('',#7732,1.);
#2219=VECTOR('',#7733,1.);
#2220=VECTOR('',#7734,1.);
#2221=VECTOR('',#7735,1.);
#2222=VECTOR('',#7758,1.);
#2223=VECTOR('',#7759,1.);
#2224=VECTOR('',#7770,0.15);
#2225=VECTOR('',#7777,0.15);
#2226=VECTOR('',#7782,0.15);
#2227=VECTOR('',#7787,0.15);
#2228=VECTOR('',#7794,0.3);
#2229=VECTOR('',#7805,0.3);
#2230=VECTOR('',#7814,0.17);
#2231=VECTOR('',#7819,0.17);
#2232=VECTOR('',#7824,1.);
#2233=VECTOR('',#7825,1.);
#2234=VECTOR('',#7826,1.);
#2235=VECTOR('',#7827,1.);
#2236=VECTOR('',#7830,1.);
#2237=VECTOR('',#7831,1.);
#2238=VECTOR('',#7832,1.);
#2239=VECTOR('',#7833,1.);
#2240=VECTOR('',#7836,1.);
#2241=VECTOR('',#7837,1.);
#2242=VECTOR('',#7838,1.);
#2243=VECTOR('',#7839,1.);
#2244=VECTOR('',#7842,1.);
#2245=VECTOR('',#7843,1.);
#2246=VECTOR('',#7844,1.);
#2247=VECTOR('',#7845,1.);
#2248=VECTOR('',#7848,1.);
#2249=VECTOR('',#7849,1.);
#2250=VECTOR('',#7850,1.);
#2251=VECTOR('',#7851,1.);
#2252=VECTOR('',#7854,1.);
#2253=VECTOR('',#7855,1.);
#2254=VECTOR('',#7856,1.);
#2255=VECTOR('',#7857,1.);
#2256=VECTOR('',#7860,1.);
#2257=VECTOR('',#7861,1.);
#2258=VECTOR('',#7862,1.);
#2259=VECTOR('',#7863,1.);
#2260=VECTOR('',#7874,1.);
#2261=VECTOR('',#7875,1.);
#2262=VECTOR('',#7878,1.);
#2263=VECTOR('',#7879,1.);
#2264=VECTOR('',#7882,1.);
#2265=VECTOR('',#7883,1.);
#2266=VECTOR('',#7886,1.);
#2267=VECTOR('',#7887,1.);
#2268=VECTOR('',#7888,1.);
#2269=VECTOR('',#7891,1.);
#2270=VECTOR('',#7892,1.);
#2271=VECTOR('',#7893,1.);
#2272=VECTOR('',#7896,1.);
#2273=VECTOR('',#7897,1.);
#2274=VECTOR('',#7900,1.);
#2275=VECTOR('',#7901,1.);
#2276=VECTOR('',#7902,1.);
#2277=VECTOR('',#7905,1.);
#2278=VECTOR('',#7906,1.);
#2279=VECTOR('',#7907,1.);
#2280=VECTOR('',#7910,1.);
#2281=VECTOR('',#7911,1.);
#2282=VECTOR('',#7914,1.);
#2283=VECTOR('',#7915,1.);
#2284=VECTOR('',#7916,1.);
#2285=VECTOR('',#7919,1.);
#2286=VECTOR('',#7920,1.);
#2287=VECTOR('',#7921,1.);
#2288=VECTOR('',#7922,1.);
#2289=VECTOR('',#7923,1.);
#2290=VECTOR('',#7924,1.);
#2291=VECTOR('',#7925,1.);
#2292=VECTOR('',#7926,1.);
#2293=VECTOR('',#7927,1.);
#2294=VECTOR('',#7928,1.);
#2295=VECTOR('',#7929,1.);
#2296=VECTOR('',#7934,0.4);
#2297=VECTOR('',#7937,0.4);
#2298=VECTOR('',#7940,1.);
#2299=VECTOR('',#7947,1.);
#2300=VECTOR('',#7950,1.);
#2301=VECTOR('',#7957,1.);
#2302=VECTOR('',#7962,1.);
#2303=VECTOR('',#7995,1.);
#2304=VECTOR('',#8024,1.);
#2305=VECTOR('',#8025,1.);
#2306=VECTOR('',#8036,1.);
#2307=VECTOR('',#8037,1.);
#2308=VECTOR('',#8048,1.);
#2309=VECTOR('',#8049,1.);
#2310=VECTOR('',#8060,0.15);
#2311=VECTOR('',#8067,0.15);
#2312=VECTOR('',#8072,0.15);
#2313=VECTOR('',#8077,0.15);
#2314=VECTOR('',#8082,1.);
#2315=VECTOR('',#8083,1.);
#2316=VECTOR('',#8084,1.);
#2317=VECTOR('',#8085,1.);
#2318=VECTOR('',#8088,1.);
#2319=VECTOR('',#8089,1.);
#2320=VECTOR('',#8090,1.);
#2321=VECTOR('',#8093,1.);
#2322=VECTOR('',#8094,1.);
#2323=VECTOR('',#8095,1.);
#2324=VECTOR('',#8098,1.);
#2325=VECTOR('',#8099,1.);
#2326=VECTOR('',#8100,1.);
#2327=VECTOR('',#8103,1.);
#2328=VECTOR('',#8104,1.);
#2329=VECTOR('',#8105,1.);
#2330=VECTOR('',#8108,1.);
#2331=VECTOR('',#8109,1.);
#2332=VECTOR('',#8116,1.);
#2333=VECTOR('',#8117,1.);
#2334=VECTOR('',#8118,1.);
#2335=VECTOR('',#8119,1.);
#2336=VECTOR('',#8122,1.);
#2337=VECTOR('',#8123,1.);
#2338=VECTOR('',#8124,1.);
#2339=VECTOR('',#8127,1.);
#2340=VECTOR('',#8128,1.);
#2341=VECTOR('',#8129,1.);
#2342=VECTOR('',#8132,1.);
#2343=VECTOR('',#8133,1.);
#2344=VECTOR('',#8134,1.);
#2345=VECTOR('',#8137,1.);
#2346=VECTOR('',#8138,1.);
#2347=VECTOR('',#8139,1.);
#2348=VECTOR('',#8142,1.);
#2349=VECTOR('',#8143,1.);
#2350=VECTOR('',#8150,0.17);
#2351=VECTOR('',#8155,0.17);
#2352=VECTOR('',#8160,1.);
#2353=VECTOR('',#8161,1.);
#2354=VECTOR('',#8162,1.);
#2355=VECTOR('',#8163,1.);
#2356=VECTOR('',#8166,1.);
#2357=VECTOR('',#8167,1.);
#2358=VECTOR('',#8168,1.);
#2359=VECTOR('',#8169,1.);
#2360=VECTOR('',#8172,1.);
#2361=VECTOR('',#8173,1.);
#2362=VECTOR('',#8174,1.);
#2363=VECTOR('',#8175,1.);
#2364=VECTOR('',#8178,1.);
#2365=VECTOR('',#8179,1.);
#2366=VECTOR('',#8180,1.);
#2367=VECTOR('',#8181,1.);
#2368=VECTOR('',#8184,1.);
#2369=VECTOR('',#8185,1.);
#2370=VECTOR('',#8186,1.);
#2371=VECTOR('',#8187,1.);
#2372=VECTOR('',#8190,1.);
#2373=VECTOR('',#8191,1.);
#2374=VECTOR('',#8192,1.);
#2375=VECTOR('',#8193,1.);
#2376=VECTOR('',#8196,1.);
#2377=VECTOR('',#8197,1.);
#2378=VECTOR('',#8198,1.);
#2379=VECTOR('',#8199,1.);
#2380=VECTOR('',#8210,1.);
#2381=VECTOR('',#8211,1.);
#2382=VECTOR('',#8214,1.);
#2383=VECTOR('',#8215,1.);
#2384=VECTOR('',#8218,1.);
#2385=VECTOR('',#8219,1.);
#2386=VECTOR('',#8222,1.);
#2387=VECTOR('',#8223,1.);
#2388=VECTOR('',#8224,1.);
#2389=VECTOR('',#8227,1.);
#2390=VECTOR('',#8228,1.);
#2391=VECTOR('',#8229,1.);
#2392=VECTOR('',#8232,1.);
#2393=VECTOR('',#8233,1.);
#2394=VECTOR('',#8236,1.);
#2395=VECTOR('',#8237,1.);
#2396=VECTOR('',#8238,1.);
#2397=VECTOR('',#8241,1.);
#2398=VECTOR('',#8242,1.);
#2399=VECTOR('',#8243,1.);
#2400=VECTOR('',#8246,1.);
#2401=VECTOR('',#8247,1.);
#2402=VECTOR('',#8250,1.);
#2403=VECTOR('',#8251,1.);
#2404=VECTOR('',#8252,1.);
#2405=VECTOR('',#8255,1.);
#2406=VECTOR('',#8256,1.);
#2407=VECTOR('',#8257,1.);
#2408=VECTOR('',#8258,1.);
#2409=VECTOR('',#8259,1.);
#2410=VECTOR('',#8260,1.);
#2411=VECTOR('',#8261,1.);
#2412=VECTOR('',#8262,1.);
#2413=VECTOR('',#8263,1.);
#2414=VECTOR('',#8264,1.);
#2415=VECTOR('',#8265,1.);
#2416=VECTOR('',#8270,0.4);
#2417=VECTOR('',#8273,0.4);
#2418=VECTOR('',#8276,1.);
#2419=VECTOR('',#8283,1.);
#2420=VECTOR('',#8286,1.);
#2421=VECTOR('',#8293,1.);
#2422=VECTOR('',#8298,1.);
#2423=VECTOR('',#8331,1.);
#2424=VECTOR('',#8360,1.);
#2425=VECTOR('',#8361,1.);
#2426=VECTOR('',#8372,1.);
#2427=VECTOR('',#8373,1.);
#2428=VECTOR('',#8386,0.35);
#2429=VECTOR('',#8393,0.35);
#2430=VECTOR('',#8406,0.25);
#2431=VECTOR('',#8419,0.25);
#2432=VECTOR('',#8432,0.25);
#2433=VECTOR('',#8445,0.25);
#2434=VECTOR('',#8450,0.15);
#2435=VECTOR('',#8455,0.15);
#2436=VECTOR('',#8460,0.15);
#2437=VECTOR('',#8465,0.15);
#2438=VECTOR('',#8476,1.);
#2439=VECTOR('',#8477,1.);
#2440=VECTOR('',#8488,1.);
#2441=VECTOR('',#8489,1.);
#2442=VECTOR('',#8494,1.);
#2443=VECTOR('',#8499,1.);
#2444=VECTOR('',#8506,0.15);
#2445=VECTOR('',#8511,0.15);
#2446=VECTOR('',#8514,0.15);
#2447=VECTOR('',#8517,0.15);
#2448=VECTOR('',#8520,0.15);
#2449=VECTOR('',#8523,0.15);
#2450=VECTOR('',#8526,0.15);
#2451=VECTOR('',#8529,0.15);
#2452=VECTOR('',#8532,0.15);
#2453=VECTOR('',#8535,0.15);
#2454=VECTOR('',#8538,0.15);
#2455=VECTOR('',#8541,0.15);
#2456=VECTOR('',#8544,0.15);
#2457=VECTOR('',#8547,0.15);
#2458=VECTOR('',#8550,0.15);
#2459=VECTOR('',#8553,0.15);
#2460=VECTOR('',#8556,0.15);
#2461=VECTOR('',#8559,0.15);
#2462=VECTOR('',#8562,0.15);
#2463=VECTOR('',#8565,0.15);
#2464=VECTOR('',#8568,0.15);
#2465=VECTOR('',#8571,0.15);
#2466=VECTOR('',#8574,0.15);
#2467=VECTOR('',#8577,0.15);
#2468=VECTOR('',#8580,0.15);
#2469=VECTOR('',#8583,0.15);
#2470=VECTOR('',#8586,0.15);
#2471=VECTOR('',#8589,0.15);
#2472=VECTOR('',#8592,0.15);
#2473=VECTOR('',#8595,0.15);
#2474=VECTOR('',#8598,0.117775);
#2475=VECTOR('',#8603,0.117775);
#2476=VECTOR('',#8606,0.117775);
#2477=VECTOR('',#8609,0.117775);
#2478=VECTOR('',#8612,0.117775);
#2479=VECTOR('',#8615,0.117775);
#2480=VECTOR('',#8618,0.117775);
#2481=VECTOR('',#8621,0.117775);
#2482=VECTOR('',#8624,0.117775);
#2483=VECTOR('',#8627,0.117775);
#2484=VECTOR('',#8630,0.117775);
#2485=VECTOR('',#8633,0.117775);
#2486=VECTOR('',#8636,0.117775);
#2487=VECTOR('',#8639,0.117775);
#2488=VECTOR('',#8642,0.117775);
#2489=VECTOR('',#8645,0.117775);
#2490=VECTOR('',#8648,0.117775);
#2491=VECTOR('',#8651,0.117775);
#2492=VECTOR('',#8654,0.117775);
#2493=VECTOR('',#8657,0.117775);
#2494=VECTOR('',#8660,0.117775);
#2495=VECTOR('',#8663,0.117775);
#2496=VECTOR('',#8666,0.117775);
#2497=VECTOR('',#8669,0.117775);
#2498=VECTOR('',#8672,0.117775);
#2499=VECTOR('',#8675,0.117775);
#2500=VECTOR('',#8678,0.117775);
#2501=VECTOR('',#8681,0.117775);
#2502=VECTOR('',#8684,0.117775);
#2503=VECTOR('',#8687,0.117775);
#2504=VECTOR('',#8692,0.1);
#2505=VECTOR('',#8703,1.);
#2506=VECTOR('',#8704,1.);
#2507=VECTOR('',#8705,1.);
#2508=VECTOR('',#8706,1.);
#2509=VECTOR('',#8709,1.);
#2510=VECTOR('',#8710,1.);
#2511=VECTOR('',#8711,1.);
#2512=VECTOR('',#8714,1.);
#2513=VECTOR('',#8715,1.);
#2514=VECTOR('',#8716,1.);
#2515=VECTOR('',#8719,1.);
#2516=VECTOR('',#8720,1.);
#2517=VECTOR('',#8721,1.);
#2518=VECTOR('',#8724,1.);
#2519=VECTOR('',#8725,1.);
#2520=VECTOR('',#8726,1.);
#2521=VECTOR('',#8729,1.);
#2522=VECTOR('',#8730,1.);
#2523=VECTOR('',#8739,0.275);
#2524=VECTOR('',#8750,0.15);
#2525=VECTOR('',#8755,0.15);
#2526=VECTOR('',#8760,0.15);
#2527=VECTOR('',#8763,0.15);
#2528=VECTOR('',#8766,0.15);
#2529=VECTOR('',#8771,0.1543);
#2530=VECTOR('',#8776,0.1543);
#2531=VECTOR('',#8779,0.1543);
#2532=VECTOR('',#8782,0.1543);
#2533=VECTOR('',#8785,0.1543);
#2534=VECTOR('',#8792,1.);
#2535=VECTOR('',#8793,1.);
#2536=VECTOR('',#8794,1.);
#2537=VECTOR('',#8795,1.);
#2538=VECTOR('',#8796,1.);
#2539=VECTOR('',#8797,1.);
#2540=VECTOR('',#8802,1.);
#2541=VECTOR('',#8803,1.);
#2542=VECTOR('',#8804,1.);
#2543=VECTOR('',#8807,1.);
#2544=VECTOR('',#8808,1.);
#2545=VECTOR('',#8811,1.);
#2546=VECTOR('',#8812,1.);
#2547=VECTOR('',#8815,1.);
#2548=VECTOR('',#8816,1.);
#2549=VECTOR('',#8819,1.);
#2550=VECTOR('',#8820,1.);
#2551=VECTOR('',#8823,1.);
#2552=VECTOR('',#8848,0.41);
#2553=VECTOR('',#8855,0.6);
#2554=CIRCLE('',#6944,0.17);
#2555=CIRCLE('',#6945,0.17);
#2556=CIRCLE('',#6947,0.17);
#2557=CIRCLE('',#6948,0.17);
#2558=CIRCLE('',#6950,0.41);
#2559=CIRCLE('',#6951,0.41);
#2560=CIRCLE('',#6960,1.4);
#2561=CIRCLE('',#6961,1.4);
#2562=CIRCLE('',#6970,1.4);
#2563=CIRCLE('',#6971,1.4);
#2564=CIRCLE('',#6982,0.17);
#2565=CIRCLE('',#6983,0.17);
#2566=CIRCLE('',#6985,0.17);
#2567=CIRCLE('',#6986,0.17);
#2568=CIRCLE('',#6988,0.41);
#2569=CIRCLE('',#6989,0.41);
#2570=CIRCLE('',#6998,1.4);
#2571=CIRCLE('',#6999,1.4);
#2572=CIRCLE('',#7001,1.4);
#2573=CIRCLE('',#7009,1.4);
#2574=CIRCLE('',#7013,0.3);
#2575=CIRCLE('',#7014,0.3);
#2576=CIRCLE('',#7016,0.4);
#2577=CIRCLE('',#7018,0.4);
#2578=CIRCLE('',#7020,0.4);
#2579=CIRCLE('',#7022,0.6);
#2580=CIRCLE('',#7023,0.4);
#2581=CIRCLE('',#7025,0.6);
#2582=CIRCLE('',#7033,0.6);
#2583=CIRCLE('',#7034,0.3);
#2584=CIRCLE('',#7036,0.3);
#2585=CIRCLE('',#7038,0.6);
#2586=CIRCLE('',#7043,0.15);
#2587=CIRCLE('',#7044,0.15);
#2588=CIRCLE('',#7045,0.4);
#2589=CIRCLE('',#7047,0.15);
#2590=CIRCLE('',#7048,0.15);
#2591=CIRCLE('',#7050,0.15);
#2592=CIRCLE('',#7052,0.15);
#2593=CIRCLE('',#7054,0.15);
#2594=CIRCLE('',#7055,0.15);
#2595=CIRCLE('',#7057,0.3);
#2596=CIRCLE('',#7058,0.3);
#2597=CIRCLE('',#7060,0.17);
#2598=CIRCLE('',#7062,0.3);
#2599=CIRCLE('',#7063,0.3);
#2600=CIRCLE('',#7065,0.17);
#2601=CIRCLE('',#7067,0.17);
#2602=CIRCLE('',#7069,0.17);
#2603=CIRCLE('',#7078,0.4);
#2604=CIRCLE('',#7080,0.4);
#2605=CIRCLE('',#7093,0.4);
#2606=CIRCLE('',#7096,0.1);
#2607=CIRCLE('',#7103,0.0999999999999999);
#2608=CIRCLE('',#7105,0.0999999999999999);
#2609=CIRCLE('',#7107,0.0999999999999999);
#2610=CIRCLE('',#7108,0.1);
#2611=CIRCLE('',#7110,0.0999999999999998);
#2612=CIRCLE('',#7111,0.0999999999999998);
#2613=CIRCLE('',#7112,0.0999999999999997);
#2614=CIRCLE('',#7114,0.0999999999999998);
#2615=CIRCLE('',#7115,0.0999999999999998);
#2616=CIRCLE('',#7118,0.0999999999999999);
#2617=CIRCLE('',#7119,0.1);
#2618=CIRCLE('',#7123,0.3);
#2619=CIRCLE('',#7124,0.3);
#2620=CIRCLE('',#7125,0.3);
#2621=CIRCLE('',#7127,0.3);
#2622=CIRCLE('',#7128,0.3);
#2623=CIRCLE('',#7129,0.3);
#2624=CIRCLE('',#7131,0.3);
#2625=CIRCLE('',#7132,0.3);
#2626=CIRCLE('',#7133,0.3);
#2627=CIRCLE('',#7136,0.3);
#2628=CIRCLE('',#7137,0.3);
#2629=CIRCLE('',#7138,0.3);
#2630=CIRCLE('',#7145,0.15);
#2631=CIRCLE('',#7146,0.15);
#2632=CIRCLE('',#7147,0.4);
#2633=CIRCLE('',#7149,0.15);
#2634=CIRCLE('',#7150,0.15);
#2635=CIRCLE('',#7152,0.15);
#2636=CIRCLE('',#7154,0.15);
#2637=CIRCLE('',#7156,0.15);
#2638=CIRCLE('',#7157,0.15);
#2639=CIRCLE('',#7165,0.17);
#2640=CIRCLE('',#7173,0.17);
#2641=CIRCLE('',#7175,0.17);
#2642=CIRCLE('',#7177,0.17);
#2643=CIRCLE('',#7186,0.4);
#2644=CIRCLE('',#7188,0.4);
#2645=CIRCLE('',#7201,0.4);
#2646=CIRCLE('',#7204,0.1);
#2647=CIRCLE('',#7211,0.0999999999999999);
#2648=CIRCLE('',#7213,0.0999999999999999);
#2649=CIRCLE('',#7215,0.0999999999999999);
#2650=CIRCLE('',#7216,0.1);
#2651=CIRCLE('',#7218,0.0999999999999998);
#2652=CIRCLE('',#7219,0.0999999999999998);
#2653=CIRCLE('',#7220,0.0999999999999997);
#2654=CIRCLE('',#7222,0.0999999999999998);
#2655=CIRCLE('',#7223,0.0999999999999998);
#2656=CIRCLE('',#7226,0.0999999999999999);
#2657=CIRCLE('',#7227,0.1);
#2658=CIRCLE('',#7231,0.3);
#2659=CIRCLE('',#7232,0.3);
#2660=CIRCLE('',#7233,0.3);
#2661=CIRCLE('',#7235,0.3);
#2662=CIRCLE('',#7236,0.3);
#2663=CIRCLE('',#7237,0.3);
#2664=CIRCLE('',#7239,0.3);
#2665=CIRCLE('',#7240,0.3);
#2666=CIRCLE('',#7241,0.3);
#2667=CIRCLE('',#7244,0.3);
#2668=CIRCLE('',#7245,0.3);
#2669=CIRCLE('',#7246,0.3);
#2670=CIRCLE('',#7253,0.35);
#2671=CIRCLE('',#7254,0.35);
#2672=CIRCLE('',#7256,0.35);
#2673=CIRCLE('',#7257,0.35);
#2674=CIRCLE('',#7259,0.25);
#2675=CIRCLE('',#7260,0.15);
#2676=CIRCLE('',#7262,0.25);
#2677=CIRCLE('',#7265,0.25);
#2678=CIRCLE('',#7266,0.15);
#2679=CIRCLE('',#7268,0.25);
#2680=CIRCLE('',#7271,0.25);
#2681=CIRCLE('',#7272,0.15);
#2682=CIRCLE('',#7274,0.25);
#2683=CIRCLE('',#7277,0.25);
#2684=CIRCLE('',#7278,0.15);
#2685=CIRCLE('',#7280,0.25);
#2686=CIRCLE('',#7283,0.15);
#2687=CIRCLE('',#7285,0.15);
#2688=CIRCLE('',#7287,0.15);
#2689=CIRCLE('',#7289,0.15);
#2690=CIRCLE('',#7290,0.0800000000000001);
#2691=CIRCLE('',#7291,0.0800000000000001);
#2692=CIRCLE('',#7293,0.0800000000000001);
#2693=CIRCLE('',#7294,0.0800000000000001);
#2694=CIRCLE('',#7295,0.0800000000000001);
#2695=CIRCLE('',#7296,0.0800000000000003);
#2696=CIRCLE('',#7298,0.0800000000000001);
#2697=CIRCLE('',#7299,0.0800000000000003);
#2698=CIRCLE('',#7306,0.14635);
#2699=CIRCLE('',#7337,0.117775);
#2700=CIRCLE('',#7368,0.14635);
#2701=CIRCLE('',#7369,0.05);
#2702=CIRCLE('',#7371,0.117775);
#2703=CIRCLE('',#7381,0.275);
#2704=CIRCLE('',#7383,0.275);
#2705=CIRCLE('',#7388,0.12645);
#2706=CIRCLE('',#7390,0.12645);
#2707=CIRCLE('',#7394,0.12645);
#2708=CIRCLE('',#7396,0.1543);
#2709=CIRCLE('',#7401,0.1543);
#2710=CIRCLE('',#7422,0.41);
#2711=CIRCLE('',#7423,0.41);
#2712=CIRCLE('',#7425,0.6);
#2713=CIRCLE('',#7426,0.6);
#2714=VERTEX_POINT('',#8881);
#2715=VERTEX_POINT('',#8883);
#2716=VERTEX_POINT('',#8887);
#2717=VERTEX_POINT('',#8889);
#2718=VERTEX_POINT('',#8893);
#2719=VERTEX_POINT('',#8895);
#2720=VERTEX_POINT('',#8899);
#2721=VERTEX_POINT('',#8900);
#2722=VERTEX_POINT('',#8902);
#2723=VERTEX_POINT('',#8906);
#2724=VERTEX_POINT('',#8907);
#2725=VERTEX_POINT('',#8912);
#2726=VERTEX_POINT('',#8916);
#2727=VERTEX_POINT('',#8918);
#2728=VERTEX_POINT('',#8920);
#2729=VERTEX_POINT('',#8922);
#2730=VERTEX_POINT('',#8924);
#2731=VERTEX_POINT('',#8928);
#2732=VERTEX_POINT('',#8932);
#2733=VERTEX_POINT('',#8936);
#2734=VERTEX_POINT('',#8940);
#2735=VERTEX_POINT('',#8942);
#2736=VERTEX_POINT('',#8944);
#2737=VERTEX_POINT('',#8946);
#2738=VERTEX_POINT('',#8948);
#2739=VERTEX_POINT('',#8950);
#2740=VERTEX_POINT('',#8952);
#2741=VERTEX_POINT('',#8954);
#2742=VERTEX_POINT('',#8956);
#2743=VERTEX_POINT('',#8958);
#2744=VERTEX_POINT('',#8960);
#2745=VERTEX_POINT('',#8962);
#2746=VERTEX_POINT('',#8966);
#2747=VERTEX_POINT('',#8968);
#2748=VERTEX_POINT('',#8972);
#2749=VERTEX_POINT('',#8974);
#2750=VERTEX_POINT('',#8976);
#2751=VERTEX_POINT('',#8982);
#2752=VERTEX_POINT('',#8984);
#2753=VERTEX_POINT('',#8994);
#2754=VERTEX_POINT('',#8996);
#2755=VERTEX_POINT('',#8998);
#2756=VERTEX_POINT('',#9000);
#2757=VERTEX_POINT('',#9002);
#2758=VERTEX_POINT('',#9004);
#2759=VERTEX_POINT('',#9006);
#2760=VERTEX_POINT('',#9026);
#2761=VERTEX_POINT('',#9028);
#2762=VERTEX_POINT('',#9032);
#2763=VERTEX_POINT('',#9034);
#2764=VERTEX_POINT('',#9038);
#2765=VERTEX_POINT('',#9040);
#2766=VERTEX_POINT('',#9044);
#2767=VERTEX_POINT('',#9045);
#2768=VERTEX_POINT('',#9047);
#2769=VERTEX_POINT('',#9049);
#2770=VERTEX_POINT('',#9053);
#2771=VERTEX_POINT('',#9055);
#2772=VERTEX_POINT('',#9057);
#2773=VERTEX_POINT('',#9061);
#2774=VERTEX_POINT('',#9062);
#2775=VERTEX_POINT('',#9064);
#2776=VERTEX_POINT('',#9069);
#2777=VERTEX_POINT('',#9070);
#2778=VERTEX_POINT('',#9072);
#2779=VERTEX_POINT('',#9074);
#2780=VERTEX_POINT('',#9078);
#2781=VERTEX_POINT('',#9082);
#2782=VERTEX_POINT('',#9089);
#2783=VERTEX_POINT('',#9091);
#2784=VERTEX_POINT('',#9093);
#2785=VERTEX_POINT('',#9095);
#2786=VERTEX_POINT('',#9097);
#2787=VERTEX_POINT('',#9099);
#2788=VERTEX_POINT('',#9101);
#2789=VERTEX_POINT('',#9105);
#2790=VERTEX_POINT('',#9109);
#2791=VERTEX_POINT('',#9111);
#2792=VERTEX_POINT('',#9115);
#2793=VERTEX_POINT('',#9119);
#2794=VERTEX_POINT('',#9123);
#2795=VERTEX_POINT('',#9127);
#2796=VERTEX_POINT('',#9137);
#2797=VERTEX_POINT('',#9139);
#2798=VERTEX_POINT('',#9143);
#2799=VERTEX_POINT('',#9146);
#2800=VERTEX_POINT('',#9149);
#2801=VERTEX_POINT('',#9153);
#2802=VERTEX_POINT('',#9155);
#2803=VERTEX_POINT('',#9158);
#2804=VERTEX_POINT('',#9167);
#2805=VERTEX_POINT('',#9168);
#2806=VERTEX_POINT('',#9170);
#2807=VERTEX_POINT('',#9172);
#2808=VERTEX_POINT('',#9176);
#2809=VERTEX_POINT('',#9177);
#2810=VERTEX_POINT('',#9179);
#2811=VERTEX_POINT('',#9181);
#2812=VERTEX_POINT('',#9195);
#2813=VERTEX_POINT('',#9196);
#2814=VERTEX_POINT('',#9201);
#2815=VERTEX_POINT('',#9203);
#2816=VERTEX_POINT('',#9208);
#2817=VERTEX_POINT('',#9228);
#2818=VERTEX_POINT('',#9233);
#2819=VERTEX_POINT('',#9235);
#2820=VERTEX_POINT('',#9259);
#2821=VERTEX_POINT('',#9261);
#2822=VERTEX_POINT('',#9263);
#2823=VERTEX_POINT('',#9266);
#2824=VERTEX_POINT('',#9268);
#2825=VERTEX_POINT('',#9272);
#2826=VERTEX_POINT('',#9276);
#2827=VERTEX_POINT('',#9280);
#2828=VERTEX_POINT('',#9282);
#2829=VERTEX_POINT('',#9286);
#2830=VERTEX_POINT('',#9288);
#2831=VERTEX_POINT('',#9292);
#2832=VERTEX_POINT('',#9295);
#2833=VERTEX_POINT('',#9297);
#2834=VERTEX_POINT('',#9301);
#2835=VERTEX_POINT('',#9304);
#2836=VERTEX_POINT('',#9308);
#2837=VERTEX_POINT('',#9312);
#2838=VERTEX_POINT('',#9313);
#2839=VERTEX_POINT('',#9315);
#2840=VERTEX_POINT('',#9317);
#2841=VERTEX_POINT('',#9321);
#2842=VERTEX_POINT('',#9322);
#2843=VERTEX_POINT('',#9324);
#2844=VERTEX_POINT('',#9326);
#2845=VERTEX_POINT('',#9330);
#2846=VERTEX_POINT('',#9331);
#2847=VERTEX_POINT('',#9333);
#2848=VERTEX_POINT('',#9335);
#2849=VERTEX_POINT('',#9339);
#2850=VERTEX_POINT('',#9340);
#2851=VERTEX_POINT('',#9342);
#2852=VERTEX_POINT('',#9344);
#2853=VERTEX_POINT('',#9348);
#2854=VERTEX_POINT('',#9349);
#2855=VERTEX_POINT('',#9351);
#2856=VERTEX_POINT('',#9353);
#2857=VERTEX_POINT('',#9357);
#2858=VERTEX_POINT('',#9358);
#2859=VERTEX_POINT('',#9360);
#2860=VERTEX_POINT('',#9362);
#2861=VERTEX_POINT('',#9366);
#2862=VERTEX_POINT('',#9367);
#2863=VERTEX_POINT('',#9369);
#2864=VERTEX_POINT('',#9371);
#2865=VERTEX_POINT('',#9375);
#2866=VERTEX_POINT('',#9378);
#2867=VERTEX_POINT('',#9390);
#2868=VERTEX_POINT('',#9392);
#2869=VERTEX_POINT('',#9396);
#2870=VERTEX_POINT('',#9398);
#2871=VERTEX_POINT('',#9402);
#2872=VERTEX_POINT('',#9403);
#2873=VERTEX_POINT('',#9405);
#2874=VERTEX_POINT('',#9412);
#2875=VERTEX_POINT('',#9441);
#2876=VERTEX_POINT('',#9443);
#2877=VERTEX_POINT('',#9479);
#2878=VERTEX_POINT('',#9481);
#2879=VERTEX_POINT('',#9488);
#2880=VERTEX_POINT('',#9517);
#2881=VERTEX_POINT('',#9519);
#2882=VERTEX_POINT('',#9548);
#2883=VERTEX_POINT('',#9557);
#2884=VERTEX_POINT('',#9559);
#2885=VERTEX_POINT('',#9566);
#2886=VERTEX_POINT('',#9595);
#2887=VERTEX_POINT('',#9597);
#2888=VERTEX_POINT('',#9626);
#2889=VERTEX_POINT('',#9635);
#2890=VERTEX_POINT('',#9637);
#2891=VERTEX_POINT('',#9672);
#2892=VERTEX_POINT('',#9701);
#2893=VERTEX_POINT('',#9710);
#2894=VERTEX_POINT('',#9712);
#2895=VERTEX_POINT('',#9717);
#2896=VERTEX_POINT('',#9719);
#2897=VERTEX_POINT('',#9734);
#2898=VERTEX_POINT('',#9746);
#2899=VERTEX_POINT('',#9752);
#2900=VERTEX_POINT('',#9754);
#2901=VERTEX_POINT('',#9787);
#2902=VERTEX_POINT('',#9789);
#2903=VERTEX_POINT('',#9827);
#2904=VERTEX_POINT('',#9832);
#2905=VERTEX_POINT('',#9876);
#2906=VERTEX_POINT('',#9878);
#2907=VERTEX_POINT('',#9922);
#2908=VERTEX_POINT('',#9927);
#2909=VERTEX_POINT('',#9966);
#2910=VERTEX_POINT('',#9995);
#2911=VERTEX_POINT('',#10001);
#2912=VERTEX_POINT('',#10007);
#2913=VERTEX_POINT('',#10019);
#2914=VERTEX_POINT('',#10020);
#2915=VERTEX_POINT('',#10025);
#2916=VERTEX_POINT('',#10060);
#2917=VERTEX_POINT('',#10062);
#2918=VERTEX_POINT('',#10097);
#2919=VERTEX_POINT('',#10104);
#2920=VERTEX_POINT('',#10110);
#2921=VERTEX_POINT('',#10117);
#2922=VERTEX_POINT('',#10124);
#2923=VERTEX_POINT('',#10153);
#2924=VERTEX_POINT('',#10219);
#2925=VERTEX_POINT('',#10272);
#2926=VERTEX_POINT('',#10284);
#2927=VERTEX_POINT('',#10346);
#2928=VERTEX_POINT('',#10356);
#2929=VERTEX_POINT('',#10363);
#2930=VERTEX_POINT('',#10392);
#2931=VERTEX_POINT('',#10394);
#2932=VERTEX_POINT('',#10519);
#2933=VERTEX_POINT('',#10554);
#2934=VERTEX_POINT('',#10670);
#2935=VERTEX_POINT('',#10677);
#2936=VERTEX_POINT('',#10706);
#2937=VERTEX_POINT('',#10708);
#2938=VERTEX_POINT('',#10759);
#2939=VERTEX_POINT('',#10788);
#2940=VERTEX_POINT('',#10795);
#2941=VERTEX_POINT('',#10817);
#2942=VERTEX_POINT('',#10852);
#2943=VERTEX_POINT('',#10880);
#2944=VERTEX_POINT('',#10983);
#2945=VERTEX_POINT('',#10984);
#2946=VERTEX_POINT('',#10986);
#2947=VERTEX_POINT('',#10990);
#2948=VERTEX_POINT('',#10991);
#2949=VERTEX_POINT('',#10993);
#2950=VERTEX_POINT('',#10997);
#2951=VERTEX_POINT('',#10998);
#2952=VERTEX_POINT('',#11000);
#2953=VERTEX_POINT('',#11035);
#2954=VERTEX_POINT('',#11036);
#2955=VERTEX_POINT('',#11038);
#2956=VERTEX_POINT('',#11243);
#2957=VERTEX_POINT('',#11244);
#2958=VERTEX_POINT('',#11249);
#2959=VERTEX_POINT('',#11251);
#2960=VERTEX_POINT('',#11256);
#2961=VERTEX_POINT('',#11276);
#2962=VERTEX_POINT('',#11281);
#2963=VERTEX_POINT('',#11283);
#2964=VERTEX_POINT('',#11307);
#2965=VERTEX_POINT('',#11309);
#2966=VERTEX_POINT('',#11311);
#2967=VERTEX_POINT('',#11314);
#2968=VERTEX_POINT('',#11316);
#2969=VERTEX_POINT('',#11320);
#2970=VERTEX_POINT('',#11324);
#2971=VERTEX_POINT('',#11328);
#2972=VERTEX_POINT('',#11330);
#2973=VERTEX_POINT('',#11334);
#2974=VERTEX_POINT('',#11335);
#2975=VERTEX_POINT('',#11337);
#2976=VERTEX_POINT('',#11339);
#2977=VERTEX_POINT('',#11343);
#2978=VERTEX_POINT('',#11345);
#2979=VERTEX_POINT('',#11349);
#2980=VERTEX_POINT('',#11351);
#2981=VERTEX_POINT('',#11355);
#2982=VERTEX_POINT('',#11357);
#2983=VERTEX_POINT('',#11361);
#2984=VERTEX_POINT('',#11363);
#2985=VERTEX_POINT('',#11370);
#2986=VERTEX_POINT('',#11373);
#2987=VERTEX_POINT('',#11374);
#2988=VERTEX_POINT('',#11376);
#2989=VERTEX_POINT('',#11378);
#2990=VERTEX_POINT('',#11382);
#2991=VERTEX_POINT('',#11384);
#2992=VERTEX_POINT('',#11388);
#2993=VERTEX_POINT('',#11390);
#2994=VERTEX_POINT('',#11394);
#2995=VERTEX_POINT('',#11396);
#2996=VERTEX_POINT('',#11400);
#2997=VERTEX_POINT('',#11402);
#2998=VERTEX_POINT('',#11409);
#2999=VERTEX_POINT('',#11412);
#3000=VERTEX_POINT('',#11416);
#3001=VERTEX_POINT('',#11420);
#3002=VERTEX_POINT('',#11421);
#3003=VERTEX_POINT('',#11423);
#3004=VERTEX_POINT('',#11425);
#3005=VERTEX_POINT('',#11429);
#3006=VERTEX_POINT('',#11430);
#3007=VERTEX_POINT('',#11432);
#3008=VERTEX_POINT('',#11434);
#3009=VERTEX_POINT('',#11438);
#3010=VERTEX_POINT('',#11439);
#3011=VERTEX_POINT('',#11441);
#3012=VERTEX_POINT('',#11443);
#3013=VERTEX_POINT('',#11447);
#3014=VERTEX_POINT('',#11448);
#3015=VERTEX_POINT('',#11450);
#3016=VERTEX_POINT('',#11452);
#3017=VERTEX_POINT('',#11456);
#3018=VERTEX_POINT('',#11457);
#3019=VERTEX_POINT('',#11459);
#3020=VERTEX_POINT('',#11461);
#3021=VERTEX_POINT('',#11465);
#3022=VERTEX_POINT('',#11466);
#3023=VERTEX_POINT('',#11468);
#3024=VERTEX_POINT('',#11470);
#3025=VERTEX_POINT('',#11474);
#3026=VERTEX_POINT('',#11475);
#3027=VERTEX_POINT('',#11477);
#3028=VERTEX_POINT('',#11479);
#3029=VERTEX_POINT('',#11483);
#3030=VERTEX_POINT('',#11486);
#3031=VERTEX_POINT('',#11498);
#3032=VERTEX_POINT('',#11500);
#3033=VERTEX_POINT('',#11504);
#3034=VERTEX_POINT('',#11506);
#3035=VERTEX_POINT('',#11510);
#3036=VERTEX_POINT('',#11511);
#3037=VERTEX_POINT('',#11513);
#3038=VERTEX_POINT('',#11520);
#3039=VERTEX_POINT('',#11549);
#3040=VERTEX_POINT('',#11551);
#3041=VERTEX_POINT('',#11587);
#3042=VERTEX_POINT('',#11589);
#3043=VERTEX_POINT('',#11596);
#3044=VERTEX_POINT('',#11625);
#3045=VERTEX_POINT('',#11627);
#3046=VERTEX_POINT('',#11656);
#3047=VERTEX_POINT('',#11665);
#3048=VERTEX_POINT('',#11667);
#3049=VERTEX_POINT('',#11674);
#3050=VERTEX_POINT('',#11703);
#3051=VERTEX_POINT('',#11705);
#3052=VERTEX_POINT('',#11734);
#3053=VERTEX_POINT('',#11743);
#3054=VERTEX_POINT('',#11745);
#3055=VERTEX_POINT('',#11780);
#3056=VERTEX_POINT('',#11809);
#3057=VERTEX_POINT('',#11818);
#3058=VERTEX_POINT('',#11820);
#3059=VERTEX_POINT('',#11825);
#3060=VERTEX_POINT('',#11827);
#3061=VERTEX_POINT('',#11842);
#3062=VERTEX_POINT('',#11854);
#3063=VERTEX_POINT('',#11860);
#3064=VERTEX_POINT('',#11862);
#3065=VERTEX_POINT('',#11895);
#3066=VERTEX_POINT('',#11897);
#3067=VERTEX_POINT('',#11935);
#3068=VERTEX_POINT('',#11940);
#3069=VERTEX_POINT('',#11984);
#3070=VERTEX_POINT('',#11986);
#3071=VERTEX_POINT('',#12030);
#3072=VERTEX_POINT('',#12035);
#3073=VERTEX_POINT('',#12074);
#3074=VERTEX_POINT('',#12103);
#3075=VERTEX_POINT('',#12109);
#3076=VERTEX_POINT('',#12115);
#3077=VERTEX_POINT('',#12127);
#3078=VERTEX_POINT('',#12128);
#3079=VERTEX_POINT('',#12133);
#3080=VERTEX_POINT('',#12168);
#3081=VERTEX_POINT('',#12170);
#3082=VERTEX_POINT('',#12205);
#3083=VERTEX_POINT('',#12212);
#3084=VERTEX_POINT('',#12218);
#3085=VERTEX_POINT('',#12225);
#3086=VERTEX_POINT('',#12232);
#3087=VERTEX_POINT('',#12261);
#3088=VERTEX_POINT('',#12327);
#3089=VERTEX_POINT('',#12380);
#3090=VERTEX_POINT('',#12392);
#3091=VERTEX_POINT('',#12454);
#3092=VERTEX_POINT('',#12464);
#3093=VERTEX_POINT('',#12471);
#3094=VERTEX_POINT('',#12500);
#3095=VERTEX_POINT('',#12502);
#3096=VERTEX_POINT('',#12627);
#3097=VERTEX_POINT('',#12662);
#3098=VERTEX_POINT('',#12778);
#3099=VERTEX_POINT('',#12785);
#3100=VERTEX_POINT('',#12814);
#3101=VERTEX_POINT('',#12816);
#3102=VERTEX_POINT('',#12867);
#3103=VERTEX_POINT('',#12896);
#3104=VERTEX_POINT('',#12903);
#3105=VERTEX_POINT('',#12925);
#3106=VERTEX_POINT('',#12960);
#3107=VERTEX_POINT('',#12988);
#3108=VERTEX_POINT('',#13091);
#3109=VERTEX_POINT('',#13092);
#3110=VERTEX_POINT('',#13094);
#3111=VERTEX_POINT('',#13098);
#3112=VERTEX_POINT('',#13099);
#3113=VERTEX_POINT('',#13101);
#3114=VERTEX_POINT('',#13105);
#3115=VERTEX_POINT('',#13106);
#3116=VERTEX_POINT('',#13108);
#3117=VERTEX_POINT('',#13143);
#3118=VERTEX_POINT('',#13144);
#3119=VERTEX_POINT('',#13146);
#3120=VERTEX_POINT('',#13351);
#3121=VERTEX_POINT('',#13353);
#3122=VERTEX_POINT('',#13357);
#3123=VERTEX_POINT('',#13359);
#3124=VERTEX_POINT('',#13363);
#3125=VERTEX_POINT('',#13365);
#3126=VERTEX_POINT('',#13368);
#3127=VERTEX_POINT('',#13373);
#3128=VERTEX_POINT('',#13375);
#3129=VERTEX_POINT('',#13378);
#3130=VERTEX_POINT('',#13383);
#3131=VERTEX_POINT('',#13385);
#3132=VERTEX_POINT('',#13388);
#3133=VERTEX_POINT('',#13393);
#3134=VERTEX_POINT('',#13395);
#3135=VERTEX_POINT('',#13398);
#3136=VERTEX_POINT('',#13403);
#3137=VERTEX_POINT('',#13407);
#3138=VERTEX_POINT('',#13411);
#3139=VERTEX_POINT('',#13415);
#3140=VERTEX_POINT('',#13443);
#3141=VERTEX_POINT('',#13444);
#3142=VERTEX_POINT('',#13446);
#3143=VERTEX_POINT('',#13452);
#3144=VERTEX_POINT('',#13460);
#3145=VERTEX_POINT('',#13461);
#3146=VERTEX_POINT('',#13490);
#3147=VERTEX_POINT('',#13491);
#3148=VERTEX_POINT('',#13528);
#3149=VERTEX_POINT('',#13529);
#3150=VERTEX_POINT('',#13566);
#3151=VERTEX_POINT('',#13567);
#3152=VERTEX_POINT('',#13580);
#3153=VERTEX_POINT('',#13581);
#3154=VERTEX_POINT('',#13610);
#3155=VERTEX_POINT('',#13611);
#3156=VERTEX_POINT('',#13659);
#3157=VERTEX_POINT('',#13664);
#3158=VERTEX_POINT('',#13690);
#3159=VERTEX_POINT('',#13739);
#3160=VERTEX_POINT('',#13772);
#3161=VERTEX_POINT('',#13813);
#3162=VERTEX_POINT('',#13839);
#3163=VERTEX_POINT('',#13896);
#3164=VERTEX_POINT('',#13958);
#3165=VERTEX_POINT('',#13959);
#3166=VERTEX_POINT('',#13961);
#3167=VERTEX_POINT('',#13972);
#3168=VERTEX_POINT('',#13982);
#3169=VERTEX_POINT('',#13983);
#3170=VERTEX_POINT('',#14030);
#3171=VERTEX_POINT('',#14031);
#3172=VERTEX_POINT('',#14078);
#3173=VERTEX_POINT('',#14079);
#3174=VERTEX_POINT('',#14129);
#3175=VERTEX_POINT('',#14130);
#3176=VERTEX_POINT('',#14177);
#3177=VERTEX_POINT('',#14178);
#3178=VERTEX_POINT('',#14225);
#3179=VERTEX_POINT('',#14226);
#3180=VERTEX_POINT('',#14273);
#3181=VERTEX_POINT('',#14274);
#3182=VERTEX_POINT('',#14327);
#3183=VERTEX_POINT('',#14328);
#3184=VERTEX_POINT('',#14375);
#3185=VERTEX_POINT('',#14376);
#3186=VERTEX_POINT('',#14423);
#3187=VERTEX_POINT('',#14424);
#3188=VERTEX_POINT('',#14477);
#3189=VERTEX_POINT('',#14478);
#3190=VERTEX_POINT('',#14525);
#3191=VERTEX_POINT('',#14526);
#3192=VERTEX_POINT('',#14573);
#3193=VERTEX_POINT('',#14574);
#3194=VERTEX_POINT('',#14621);
#3195=VERTEX_POINT('',#14622);
#3196=VERTEX_POINT('',#14675);
#3197=VERTEX_POINT('',#14676);
#3198=VERTEX_POINT('',#14723);
#3199=VERTEX_POINT('',#14724);
#3200=VERTEX_POINT('',#14771);
#3201=VERTEX_POINT('',#14772);
#3202=VERTEX_POINT('',#14825);
#3203=VERTEX_POINT('',#14826);
#3204=VERTEX_POINT('',#14873);
#3205=VERTEX_POINT('',#14874);
#3206=VERTEX_POINT('',#14921);
#3207=VERTEX_POINT('',#14922);
#3208=VERTEX_POINT('',#14975);
#3209=VERTEX_POINT('',#14976);
#3210=VERTEX_POINT('',#15023);
#3211=VERTEX_POINT('',#15024);
#3212=VERTEX_POINT('',#15071);
#3213=VERTEX_POINT('',#15072);
#3214=VERTEX_POINT('',#15119);
#3215=VERTEX_POINT('',#15120);
#3216=VERTEX_POINT('',#15173);
#3217=VERTEX_POINT('',#15174);
#3218=VERTEX_POINT('',#15221);
#3219=VERTEX_POINT('',#15222);
#3220=VERTEX_POINT('',#15269);
#3221=VERTEX_POINT('',#15270);
#3222=VERTEX_POINT('',#15323);
#3223=VERTEX_POINT('',#15324);
#3224=VERTEX_POINT('',#15371);
#3225=VERTEX_POINT('',#15372);
#3226=VERTEX_POINT('',#15419);
#3227=VERTEX_POINT('',#15420);
#3228=VERTEX_POINT('',#15422);
#3229=VERTEX_POINT('',#15433);
#3230=VERTEX_POINT('',#15445);
#3231=VERTEX_POINT('',#15446);
#3232=VERTEX_POINT('',#15469);
#3233=VERTEX_POINT('',#15470);
#3234=VERTEX_POINT('',#15493);
#3235=VERTEX_POINT('',#15494);
#3236=VERTEX_POINT('',#15518);
#3237=VERTEX_POINT('',#15519);
#3238=VERTEX_POINT('',#15543);
#3239=VERTEX_POINT('',#15544);
#3240=VERTEX_POINT('',#15567);
#3241=VERTEX_POINT('',#15568);
#3242=VERTEX_POINT('',#15592);
#3243=VERTEX_POINT('',#15593);
#3244=VERTEX_POINT('',#15617);
#3245=VERTEX_POINT('',#15618);
#3246=VERTEX_POINT('',#15641);
#3247=VERTEX_POINT('',#15642);
#3248=VERTEX_POINT('',#15665);
#3249=VERTEX_POINT('',#15666);
#3250=VERTEX_POINT('',#15690);
#3251=VERTEX_POINT('',#15691);
#3252=VERTEX_POINT('',#15715);
#3253=VERTEX_POINT('',#15716);
#3254=VERTEX_POINT('',#15739);
#3255=VERTEX_POINT('',#15740);
#3256=VERTEX_POINT('',#15764);
#3257=VERTEX_POINT('',#15765);
#3258=VERTEX_POINT('',#15789);
#3259=VERTEX_POINT('',#15790);
#3260=VERTEX_POINT('',#15813);
#3261=VERTEX_POINT('',#15814);
#3262=VERTEX_POINT('',#15838);
#3263=VERTEX_POINT('',#15839);
#3264=VERTEX_POINT('',#15863);
#3265=VERTEX_POINT('',#15864);
#3266=VERTEX_POINT('',#15887);
#3267=VERTEX_POINT('',#15888);
#3268=VERTEX_POINT('',#15911);
#3269=VERTEX_POINT('',#15912);
#3270=VERTEX_POINT('',#15936);
#3271=VERTEX_POINT('',#15937);
#3272=VERTEX_POINT('',#15961);
#3273=VERTEX_POINT('',#15962);
#3274=VERTEX_POINT('',#15985);
#3275=VERTEX_POINT('',#15986);
#3276=VERTEX_POINT('',#16010);
#3277=VERTEX_POINT('',#16011);
#3278=VERTEX_POINT('',#16035);
#3279=VERTEX_POINT('',#16036);
#3280=VERTEX_POINT('',#16059);
#3281=VERTEX_POINT('',#16060);
#3282=VERTEX_POINT('',#16084);
#3283=VERTEX_POINT('',#16085);
#3284=VERTEX_POINT('',#16108);
#3285=VERTEX_POINT('',#16109);
#3286=VERTEX_POINT('',#16133);
#3287=VERTEX_POINT('',#16134);
#3288=VERTEX_POINT('',#16157);
#3289=VERTEX_POINT('',#16279);
#3290=VERTEX_POINT('',#16317);
#3291=VERTEX_POINT('',#16335);
#3292=VERTEX_POINT('',#17122);
#3293=VERTEX_POINT('',#17200);
#3294=VERTEX_POINT('',#18079);
#3295=VERTEX_POINT('',#18080);
#3296=VERTEX_POINT('',#18082);
#3297=VERTEX_POINT('',#18084);
#3298=VERTEX_POINT('',#18088);
#3299=VERTEX_POINT('',#18090);
#3300=VERTEX_POINT('',#18094);
#3301=VERTEX_POINT('',#18096);
#3302=VERTEX_POINT('',#18100);
#3303=VERTEX_POINT('',#18102);
#3304=VERTEX_POINT('',#18106);
#3305=VERTEX_POINT('',#18108);
#3306=VERTEX_POINT('',#18116);
#3307=VERTEX_POINT('',#18119);
#3308=VERTEX_POINT('',#18126);
#3309=VERTEX_POINT('',#18127);
#3310=VERTEX_POINT('',#18129);
#3311=VERTEX_POINT('',#18139);
#3312=VERTEX_POINT('',#18140);
#3313=VERTEX_POINT('',#18142);
#3314=VERTEX_POINT('',#18186);
#3315=VERTEX_POINT('',#18187);
#3316=VERTEX_POINT('',#18240);
#3317=VERTEX_POINT('',#18241);
#3318=VERTEX_POINT('',#18288);
#3319=VERTEX_POINT('',#18289);
#3320=VERTEX_POINT('',#18291);
#3321=VERTEX_POINT('',#18305);
#3322=VERTEX_POINT('',#18327);
#3323=VERTEX_POINT('',#18328);
#3324=VERTEX_POINT('',#18330);
#3325=VERTEX_POINT('',#18338);
#3326=VERTEX_POINT('',#18348);
#3327=VERTEX_POINT('',#18349);
#3328=VERTEX_POINT('',#18373);
#3329=VERTEX_POINT('',#18374);
#3330=VERTEX_POINT('',#18398);
#3331=VERTEX_POINT('',#18399);
#3332=VERTEX_POINT('',#18423);
#3333=VERTEX_POINT('',#18424);
#3334=VERTEX_POINT('',#18426);
#3335=VERTEX_POINT('',#18432);
#3336=VERTEX_POINT('',#18996);
#3337=VERTEX_POINT('',#18997);
#3338=VERTEX_POINT('',#18999);
#3339=VERTEX_POINT('',#19001);
#3340=VERTEX_POINT('',#19003);
#3341=VERTEX_POINT('',#19005);
#3342=VERTEX_POINT('',#19010);
#3343=VERTEX_POINT('',#19011);
#3344=VERTEX_POINT('',#19016);
#3345=VERTEX_POINT('',#19020);
#3346=VERTEX_POINT('',#19024);
#3347=VERTEX_POINT('',#19028);
#3348=VERTEX_POINT('',#19044);
#3349=VERTEX_POINT('',#19046);
#3350=VERTEX_POINT('',#19050);
#3351=VERTEX_POINT('',#19052);
#3352=EDGE_CURVE('',#2714,#2714,#2554,.T.);
#3353=EDGE_CURVE('',#2714,#2715,#1656,.T.);
#3354=EDGE_CURVE('',#2715,#2715,#2555,.T.);
#3355=EDGE_CURVE('',#2716,#2716,#2556,.T.);
#3356=EDGE_CURVE('',#2716,#2717,#1657,.T.);
#3357=EDGE_CURVE('',#2717,#2717,#2557,.T.);
#3358=EDGE_CURVE('',#2718,#2718,#2558,.T.);
#3359=EDGE_CURVE('',#2718,#2719,#1658,.T.);
#3360=EDGE_CURVE('',#2719,#2719,#2559,.T.);
#3361=EDGE_CURVE('',#2720,#2721,#1659,.T.);
#3362=EDGE_CURVE('',#2722,#2720,#1660,.T.);
#3363=EDGE_CURVE('',#2721,#2722,#1661,.T.);
#3364=EDGE_CURVE('',#2723,#2724,#1662,.T.);
#3365=EDGE_CURVE('',#2722,#2723,#1663,.T.);
#3366=EDGE_CURVE('',#2720,#2724,#1664,.T.);
#3367=EDGE_CURVE('',#2725,#2724,#1665,.T.);
#3368=EDGE_CURVE('',#2723,#2725,#1666,.T.);
#3369=EDGE_CURVE('',#2726,#2721,#1667,.T.);
#3370=EDGE_CURVE('',#2726,#2727,#1668,.T.);
#3371=EDGE_CURVE('',#2728,#2727,#1669,.T.);
#3372=EDGE_CURVE('',#2729,#2728,#1670,.T.);
#3373=EDGE_CURVE('',#2730,#2729,#1671,.T.);
#3374=EDGE_CURVE('',#2730,#2720,#1672,.T.);
#3375=EDGE_CURVE('',#2731,#2730,#1673,.T.);
#3376=EDGE_CURVE('',#2720,#2731,#1674,.T.);
#3377=EDGE_CURVE('',#2724,#2732,#1675,.T.);
#3378=EDGE_CURVE('',#2732,#2731,#1676,.T.);
#3379=EDGE_CURVE('',#2733,#2732,#1677,.T.);
#3380=EDGE_CURVE('',#2724,#2733,#1678,.T.);
#3381=EDGE_CURVE('',#2729,#2734,#2560,.T.);
#3382=EDGE_CURVE('',#2734,#2735,#1679,.T.);
#3383=EDGE_CURVE('',#2735,#2736,#1680,.T.);
#3384=EDGE_CURVE('',#2736,#2737,#1681,.T.);
#3385=EDGE_CURVE('',#2737,#2738,#1682,.T.);
#3386=EDGE_CURVE('',#2738,#2739,#1683,.T.);
#3387=EDGE_CURVE('',#2739,#2740,#1684,.T.);
#3388=EDGE_CURVE('',#2740,#2741,#2561,.T.);
#3389=EDGE_CURVE('',#2741,#2742,#1685,.T.);
#3390=EDGE_CURVE('',#2742,#2743,#1686,.T.);
#3391=EDGE_CURVE('',#2743,#2744,#1687,.T.);
#3392=EDGE_CURVE('',#2744,#2745,#1688,.T.);
#3393=EDGE_CURVE('',#2745,#2733,#1689,.T.);
#3394=EDGE_CURVE('',#2746,#2726,#1690,.T.);
#3395=EDGE_CURVE('',#2746,#2747,#1691,.T.);
#3396=EDGE_CURVE('',#2727,#2747,#1692,.T.);
#3397=EDGE_CURVE('',#2725,#2748,#1693,.T.);
#3398=EDGE_CURVE('',#2748,#2749,#1694,.T.);
#3399=EDGE_CURVE('',#2749,#2750,#1695,.T.);
#3400=EDGE_CURVE('',#2750,#2746,#1696,.T.);
#3401=EDGE_CURVE('',#2748,#2745,#1697,.T.);
#3402=EDGE_CURVE('',#2751,#2741,#1698,.T.);
#3403=EDGE_CURVE('',#2752,#2751,#1699,.T.);
#3404=EDGE_CURVE('',#2752,#2742,#1700,.T.);
#3405=EDGE_CURVE('',#2749,#2744,#1701,.T.);
#3406=EDGE_CURVE('',#2750,#2743,#1702,.T.);
#3407=EDGE_CURVE('',#2747,#2752,#1703,.T.);
#3408=EDGE_CURVE('',#2753,#2751,#2562,.T.);
#3409=EDGE_CURVE('',#2754,#2753,#1704,.T.);
#3410=EDGE_CURVE('',#2755,#2754,#1705,.T.);
#3411=EDGE_CURVE('',#2756,#2755,#1706,.T.);
#3412=EDGE_CURVE('',#2757,#2756,#1707,.T.);
#3413=EDGE_CURVE('',#2758,#2757,#1708,.T.);
#3414=EDGE_CURVE('',#2759,#2758,#1709,.T.);
#3415=EDGE_CURVE('',#2728,#2759,#2563,.T.);
#3416=EDGE_CURVE('',#2740,#2753,#1710,.T.);
#3417=EDGE_CURVE('',#2759,#2734,#1711,.T.);
#3418=EDGE_CURVE('',#2758,#2735,#1712,.T.);
#3419=EDGE_CURVE('',#2754,#2739,#1713,.T.);
#3420=EDGE_CURVE('',#2755,#2738,#1714,.T.);
#3421=EDGE_CURVE('',#2756,#2737,#1715,.T.);
#3422=EDGE_CURVE('',#2757,#2736,#1716,.T.);
#3423=EDGE_CURVE('',#2760,#2760,#2564,.T.);
#3424=EDGE_CURVE('',#2760,#2761,#1717,.T.);
#3425=EDGE_CURVE('',#2761,#2761,#2565,.T.);
#3426=EDGE_CURVE('',#2762,#2762,#2566,.T.);
#3427=EDGE_CURVE('',#2762,#2763,#1718,.T.);
#3428=EDGE_CURVE('',#2763,#2763,#2567,.T.);
#3429=EDGE_CURVE('',#2764,#2764,#2568,.T.);
#3430=EDGE_CURVE('',#2764,#2765,#1719,.T.);
#3431=EDGE_CURVE('',#2765,#2765,#2569,.T.);
#3432=EDGE_CURVE('',#2766,#2767,#1720,.T.);
#3433=EDGE_CURVE('',#2766,#2768,#1721,.T.);
#3434=EDGE_CURVE('',#2769,#2768,#1722,.T.);
#3435=EDGE_CURVE('',#2767,#2769,#1723,.T.);
#3436=EDGE_CURVE('',#2770,#2766,#1724,.T.);
#3437=EDGE_CURVE('',#2767,#2771,#1725,.T.);
#3438=EDGE_CURVE('',#2771,#2772,#1726,.T.);
#3439=EDGE_CURVE('',#2772,#2770,#1727,.T.);
#3440=EDGE_CURVE('',#2773,#2774,#1728,.T.);
#3441=EDGE_CURVE('',#2775,#2773,#1729,.T.);
#3442=EDGE_CURVE('',#2771,#2775,#1730,.T.);
#3443=EDGE_CURVE('',#2774,#2769,#1731,.T.);
#3444=EDGE_CURVE('',#2776,#2777,#1732,.T.);
#3445=EDGE_CURVE('',#2778,#2776,#1733,.T.);
#3446=EDGE_CURVE('',#2778,#2779,#1734,.T.);
#3447=EDGE_CURVE('',#2777,#2779,#1735,.T.);
#3448=EDGE_CURVE('',#2780,#2775,#1736,.T.);
#3449=EDGE_CURVE('',#2772,#2780,#1737,.T.);
#3450=EDGE_CURVE('',#2781,#2780,#1738,.T.);
#3451=EDGE_CURVE('',#2770,#2781,#1739,.T.);
#3452=EDGE_CURVE('',#2779,#2781,#1740,.T.);
#3453=EDGE_CURVE('',#2768,#2778,#1741,.T.);
#3454=EDGE_CURVE('',#2782,#2776,#2570,.T.);
#3455=EDGE_CURVE('',#2783,#2782,#1742,.T.);
#3456=EDGE_CURVE('',#2784,#2783,#1743,.T.);
#3457=EDGE_CURVE('',#2785,#2784,#1744,.T.);
#3458=EDGE_CURVE('',#2786,#2785,#1745,.T.);
#3459=EDGE_CURVE('',#2787,#2786,#1746,.T.);
#3460=EDGE_CURVE('',#2788,#2787,#1747,.T.);
#3461=EDGE_CURVE('',#2774,#2788,#2571,.T.);
#3462=EDGE_CURVE('',#2789,#2777,#2572,.T.);
#3463=EDGE_CURVE('',#2789,#2782,#1748,.T.);
#3464=EDGE_CURVE('',#2788,#2790,#1749,.T.);
#3465=EDGE_CURVE('',#2787,#2791,#1750,.T.);
#3466=EDGE_CURVE('',#2790,#2791,#1751,.T.);
#3467=EDGE_CURVE('',#2792,#2789,#1752,.T.);
#3468=EDGE_CURVE('',#2783,#2792,#1753,.T.);
#3469=EDGE_CURVE('',#2793,#2792,#1754,.T.);
#3470=EDGE_CURVE('',#2784,#2793,#1755,.T.);
#3471=EDGE_CURVE('',#2794,#2793,#1756,.T.);
#3472=EDGE_CURVE('',#2785,#2794,#1757,.T.);
#3473=EDGE_CURVE('',#2795,#2794,#1758,.T.);
#3474=EDGE_CURVE('',#2786,#2795,#1759,.T.);
#3475=EDGE_CURVE('',#2791,#2795,#1760,.T.);
#3476=EDGE_CURVE('',#2773,#2790,#2573,.T.);
#3477=EDGE_CURVE('',#2796,#2796,#2574,.T.);
#3478=EDGE_CURVE('',#2796,#2797,#1761,.T.);
#3479=EDGE_CURVE('',#2797,#2797,#2575,.T.);
#3480=EDGE_CURVE('',#2798,#2798,#2576,.T.);
#3481=EDGE_CURVE('',#2799,#2799,#2577,.T.);
#3482=EDGE_CURVE('',#2800,#2800,#2578,.T.);
#3483=EDGE_CURVE('',#2800,#2799,#1762,.T.);
#3484=EDGE_CURVE('',#2801,#2801,#2579,.T.);
#3485=EDGE_CURVE('',#2802,#2802,#2580,.T.);
#3486=EDGE_CURVE('',#2801,#2803,#1763,.T.);
#3487=EDGE_CURVE('',#2803,#2803,#2581,.T.);
#3488=EDGE_CURVE('',#2798,#2802,#1764,.T.);
#3489=EDGE_CURVE('',#2804,#2805,#1765,.T.);
#3490=EDGE_CURVE('',#2806,#2804,#1766,.T.);
#3491=EDGE_CURVE('',#2807,#2806,#1767,.T.);
#3492=EDGE_CURVE('',#2805,#2807,#1768,.T.);
#3493=EDGE_CURVE('',#2808,#2809,#1769,.T.);
#3494=EDGE_CURVE('',#2810,#2808,#1770,.T.);
#3495=EDGE_CURVE('',#2811,#2810,#1771,.T.);
#3496=EDGE_CURVE('',#2809,#2811,#1772,.T.);
#3497=EDGE_CURVE('',#2806,#2811,#2582,.T.);
#3498=EDGE_CURVE('',#2809,#2804,#2583,.T.);
#3499=EDGE_CURVE('',#2808,#2805,#2584,.T.);
#3500=EDGE_CURVE('',#2807,#2810,#2585,.T.);
#3501=EDGE_CURVE('',#2812,#2813,#172,.T.);
#3502=EDGE_CURVE('',#2813,#2814,#1773,.T.);
#3503=EDGE_CURVE('',#2814,#2815,#173,.T.);
#3504=EDGE_CURVE('',#2816,#2815,#174,.T.);
#3505=EDGE_CURVE('',#2816,#2817,#175,.T.);
#3506=EDGE_CURVE('',#2817,#2818,#1774,.T.);
#3507=EDGE_CURVE('',#2818,#2819,#176,.T.);
#3508=EDGE_CURVE('',#2812,#2819,#177,.T.);
#3509=EDGE_CURVE('',#2820,#2820,#2586,.T.);
#3510=EDGE_CURVE('',#2821,#2821,#2587,.T.);
#3511=EDGE_CURVE('',#2822,#2822,#2588,.T.);
#3512=EDGE_CURVE('',#2823,#2823,#2589,.T.);
#3513=EDGE_CURVE('',#2823,#2824,#1775,.T.);
#3514=EDGE_CURVE('',#2824,#2824,#2590,.T.);
#3515=EDGE_CURVE('',#2825,#2825,#2591,.T.);
#3516=EDGE_CURVE('',#2825,#2821,#1776,.T.);
#3517=EDGE_CURVE('',#2826,#2826,#2592,.T.);
#3518=EDGE_CURVE('',#2826,#2820,#1777,.T.);
#3519=EDGE_CURVE('',#2827,#2827,#2593,.T.);
#3520=EDGE_CURVE('',#2827,#2828,#1778,.T.);
#3521=EDGE_CURVE('',#2828,#2828,#2594,.T.);
#3522=EDGE_CURVE('',#2829,#2829,#2595,.T.);
#3523=EDGE_CURVE('',#2829,#2830,#1779,.T.);
#3524=EDGE_CURVE('',#2830,#2830,#2596,.T.);
#3525=EDGE_CURVE('',#2831,#2831,#2597,.T.);
#3526=EDGE_CURVE('',#2832,#2832,#2598,.T.);
#3527=EDGE_CURVE('',#2832,#2833,#1780,.T.);
#3528=EDGE_CURVE('',#2833,#2833,#2599,.T.);
#3529=EDGE_CURVE('',#2834,#2834,#2600,.T.);
#3530=EDGE_CURVE('',#2831,#2835,#1781,.T.);
#3531=EDGE_CURVE('',#2835,#2835,#2601,.T.);
#3532=EDGE_CURVE('',#2834,#2836,#1782,.T.);
#3533=EDGE_CURVE('',#2836,#2836,#2602,.T.);
#3534=EDGE_CURVE('',#2837,#2838,#1783,.T.);
#3535=EDGE_CURVE('',#2839,#2837,#1784,.T.);
#3536=EDGE_CURVE('',#2840,#2839,#1785,.T.);
#3537=EDGE_CURVE('',#2840,#2838,#1786,.T.);
#3538=EDGE_CURVE('',#2841,#2842,#1787,.T.);
#3539=EDGE_CURVE('',#2841,#2843,#1788,.T.);
#3540=EDGE_CURVE('',#2844,#2843,#1789,.T.);
#3541=EDGE_CURVE('',#2842,#2844,#1790,.T.);
#3542=EDGE_CURVE('',#2845,#2846,#1791,.T.);
#3543=EDGE_CURVE('',#2845,#2847,#1792,.T.);
#3544=EDGE_CURVE('',#2848,#2847,#1793,.T.);
#3545=EDGE_CURVE('',#2846,#2848,#1794,.T.);
#3546=EDGE_CURVE('',#2849,#2850,#1795,.T.);
#3547=EDGE_CURVE('',#2849,#2851,#1796,.T.);
#3548=EDGE_CURVE('',#2852,#2851,#1797,.T.);
#3549=EDGE_CURVE('',#2850,#2852,#1798,.T.);
#3550=EDGE_CURVE('',#2853,#2854,#1799,.T.);
#3551=EDGE_CURVE('',#2853,#2855,#1800,.T.);
#3552=EDGE_CURVE('',#2856,#2855,#1801,.T.);
#3553=EDGE_CURVE('',#2854,#2856,#1802,.T.);
#3554=EDGE_CURVE('',#2857,#2858,#1803,.T.);
#3555=EDGE_CURVE('',#2859,#2857,#1804,.T.);
#3556=EDGE_CURVE('',#2860,#2859,#1805,.T.);
#3557=EDGE_CURVE('',#2860,#2858,#1806,.T.);
#3558=EDGE_CURVE('',#2861,#2862,#1807,.T.);
#3559=EDGE_CURVE('',#2863,#2861,#1808,.T.);
#3560=EDGE_CURVE('',#2864,#2863,#1809,.T.);
#3561=EDGE_CURVE('',#2864,#2862,#1810,.T.);
#3562=EDGE_CURVE('',#2865,#2865,#2603,.T.);
#3563=EDGE_CURVE('',#2866,#2866,#2604,.T.);
#3564=EDGE_CURVE('',#2838,#2853,#1811,.T.);
#3565=EDGE_CURVE('',#2855,#2840,#1812,.T.);
#3566=EDGE_CURVE('',#2858,#2841,#1813,.T.);
#3567=EDGE_CURVE('',#2843,#2860,#1814,.T.);
#3568=EDGE_CURVE('',#2862,#2845,#1815,.T.);
#3569=EDGE_CURVE('',#2847,#2864,#1816,.T.);
#3570=EDGE_CURVE('',#2867,#2849,#1817,.T.);
#3571=EDGE_CURVE('',#2868,#2867,#1818,.T.);
#3572=EDGE_CURVE('',#2851,#2868,#1819,.T.);
#3573=EDGE_CURVE('',#2869,#2867,#1820,.T.);
#3574=EDGE_CURVE('',#2870,#2869,#1821,.T.);
#3575=EDGE_CURVE('',#2868,#2870,#1822,.T.);
#3576=EDGE_CURVE('',#2871,#2872,#1823,.T.);
#3577=EDGE_CURVE('',#2873,#2872,#178,.T.);
#3578=EDGE_CURVE('',#2874,#2873,#179,.T.);
#3579=EDGE_CURVE('',#2875,#2874,#1824,.T.);
#3580=EDGE_CURVE('',#2876,#2875,#180,.T.);
#3581=EDGE_CURVE('',#2871,#2876,#181,.T.);
#3582=EDGE_CURVE('',#2870,#2877,#1825,.T.);
#3583=EDGE_CURVE('',#2878,#2877,#182,.T.);
#3584=EDGE_CURVE('',#2879,#2878,#183,.T.);
#3585=EDGE_CURVE('',#2880,#2879,#1826,.T.);
#3586=EDGE_CURVE('',#2881,#2880,#184,.T.);
#3587=EDGE_CURVE('',#2882,#2881,#185,.T.);
#3588=EDGE_CURVE('',#2882,#2852,#1827,.T.);
#3589=EDGE_CURVE('',#2863,#2883,#1828,.T.);
#3590=EDGE_CURVE('',#2884,#2883,#186,.T.);
#3591=EDGE_CURVE('',#2885,#2884,#187,.T.);
#3592=EDGE_CURVE('',#2886,#2885,#1829,.T.);
#3593=EDGE_CURVE('',#2887,#2886,#188,.T.);
#3594=EDGE_CURVE('',#2888,#2887,#189,.T.);
#3595=EDGE_CURVE('',#2888,#2848,#1830,.T.);
#3596=EDGE_CURVE('',#2859,#2889,#1831,.T.);
#3597=EDGE_CURVE('',#2890,#2889,#190,.T.);
#3598=EDGE_CURVE('',#2818,#2890,#191,.T.);
#3599=EDGE_CURVE('',#2891,#2817,#192,.T.);
#3600=EDGE_CURVE('',#2892,#2891,#193,.T.);
#3601=EDGE_CURVE('',#2892,#2844,#1832,.T.);
#3602=EDGE_CURVE('',#2893,#2854,#1833,.T.);
#3603=EDGE_CURVE('',#2893,#2894,#194,.T.);
#3604=EDGE_CURVE('',#2894,#2895,#1834,.T.);
#3605=EDGE_CURVE('',#2895,#2896,#195,.T.);
#3606=EDGE_CURVE('',#2837,#2896,#1835,.T.);
#3607=EDGE_CURVE('',#2882,#2872,#196,.T.);
#3608=EDGE_CURVE('',#2871,#2877,#197,.T.);
#3609=EDGE_CURVE('',#2897,#2869,#1836,.T.);
#3610=EDGE_CURVE('',#2897,#2883,#198,.T.);
#3611=EDGE_CURVE('',#2898,#2861,#1837,.T.);
#3612=EDGE_CURVE('',#2898,#2889,#199,.T.);
#3613=EDGE_CURVE('',#2899,#2857,#1838,.T.);
#3614=EDGE_CURVE('',#2899,#2900,#200,.T.);
#3615=EDGE_CURVE('',#2900,#2893,#201,.T.);
#3616=EDGE_CURVE('',#2856,#2901,#1839,.T.);
#3617=EDGE_CURVE('',#2902,#2901,#202,.T.);
#3618=EDGE_CURVE('',#2902,#2903,#203,.T.);
#3619=EDGE_CURVE('',#2904,#2903,#204,.T.);
#3620=EDGE_CURVE('',#2904,#2905,#1840,.T.);
#3621=EDGE_CURVE('',#2906,#2905,#205,.T.);
#3622=EDGE_CURVE('',#2906,#2907,#206,.T.);
#3623=EDGE_CURVE('',#2908,#2907,#207,.T.);
#3624=EDGE_CURVE('',#2908,#2839,#1841,.T.);
#3625=EDGE_CURVE('',#2896,#2909,#208,.T.);
#3626=EDGE_CURVE('',#2909,#2910,#209,.T.);
#3627=EDGE_CURVE('',#2842,#2910,#1842,.T.);
#3628=EDGE_CURVE('',#2892,#2911,#210,.T.);
#3629=EDGE_CURVE('',#2846,#2911,#1843,.T.);
#3630=EDGE_CURVE('',#2888,#2912,#211,.T.);
#3631=EDGE_CURVE('',#2850,#2912,#1844,.T.);
#3632=EDGE_CURVE('',#2913,#2914,#212,.T.);
#3633=EDGE_CURVE('',#2914,#2915,#213,.T.);
#3634=EDGE_CURVE('',#2915,#2916,#1845,.T.);
#3635=EDGE_CURVE('',#2916,#2917,#214,.T.);
#3636=EDGE_CURVE('',#2917,#2918,#215,.T.);
#3637=EDGE_CURVE('',#2913,#2918,#1846,.T.);
#3638=EDGE_CURVE('',#2919,#2919,#2605,.T.);
#3639=EDGE_CURVE('',#2919,#2866,#1847,.T.);
#3640=EDGE_CURVE('',#2822,#2865,#1848,.T.);
#3641=EDGE_CURVE('',#2913,#2920,#216,.T.);
#3642=EDGE_CURVE('',#2921,#2918,#217,.T.);
#3643=EDGE_CURVE('',#2922,#2921,#218,.T.);
#3644=EDGE_CURVE('',#2923,#2922,#1849,.T.);
#3645=EDGE_CURVE('',#2920,#2923,#219,.T.);
#3646=EDGE_CURVE('',#2881,#2873,#220,.T.);
#3647=EDGE_CURVE('',#2920,#2924,#221,.T.);
#3648=EDGE_CURVE('',#2924,#2914,#222,.T.);
#3649=EDGE_CURVE('',#2874,#2880,#223,.T.);
#3650=EDGE_CURVE('',#2925,#2923,#224,.T.);
#3651=EDGE_CURVE('',#2924,#2925,#2606,.F.);
#3652=EDGE_CURVE('',#2879,#2875,#225,.T.);
#3653=EDGE_CURVE('',#2922,#2926,#226,.T.);
#3654=EDGE_CURVE('',#2926,#2925,#1850,.T.);
#3655=EDGE_CURVE('',#2876,#2878,#227,.T.);
#3656=EDGE_CURVE('',#2917,#2927,#228,.T.);
#3657=EDGE_CURVE('',#2927,#2921,#229,.T.);
#3658=EDGE_CURVE('',#2928,#2912,#230,.T.);
#3659=EDGE_CURVE('',#2929,#2928,#231,.T.);
#3660=EDGE_CURVE('',#2930,#2929,#1851,.T.);
#3661=EDGE_CURVE('',#2931,#2930,#232,.T.);
#3662=EDGE_CURVE('',#2897,#2931,#233,.T.);
#3663=EDGE_CURVE('',#2887,#2928,#234,.T.);
#3664=EDGE_CURVE('',#2929,#2886,#235,.T.);
#3665=EDGE_CURVE('',#2885,#2930,#236,.T.);
#3666=EDGE_CURVE('',#2931,#2884,#237,.T.);
#3667=EDGE_CURVE('',#2932,#2911,#238,.T.);
#3668=EDGE_CURVE('',#2814,#2932,#239,.T.);
#3669=EDGE_CURVE('',#2933,#2813,#240,.T.);
#3670=EDGE_CURVE('',#2898,#2933,#241,.T.);
#3671=EDGE_CURVE('',#2891,#2932,#242,.T.);
#3672=EDGE_CURVE('',#2933,#2890,#243,.T.);
#3673=EDGE_CURVE('',#2934,#2910,#244,.T.);
#3674=EDGE_CURVE('',#2935,#2934,#245,.T.);
#3675=EDGE_CURVE('',#2936,#2935,#1852,.T.);
#3676=EDGE_CURVE('',#2937,#2936,#246,.T.);
#3677=EDGE_CURVE('',#2899,#2937,#247,.T.);
#3678=EDGE_CURVE('',#2909,#2938,#248,.T.);
#3679=EDGE_CURVE('',#2938,#2934,#249,.T.);
#3680=EDGE_CURVE('',#2939,#2938,#2607,.F.);
#3681=EDGE_CURVE('',#2935,#2939,#250,.T.);
#3682=EDGE_CURVE('',#2939,#2940,#1853,.T.);
#3683=EDGE_CURVE('',#2940,#2936,#251,.T.);
#3684=EDGE_CURVE('',#2937,#2941,#252,.T.);
#3685=EDGE_CURVE('',#2941,#2900,#253,.T.);
#3686=EDGE_CURVE('',#2941,#2940,#2608,.F.);
#3687=EDGE_CURVE('',#2940,#2894,#2609,.F.);
#3688=EDGE_CURVE('',#2894,#2941,#2610,.F.);
#3689=EDGE_CURVE('',#2926,#2927,#2611,.F.);
#3690=EDGE_CURVE('',#2927,#2942,#2612,.F.);
#3691=EDGE_CURVE('',#2942,#2926,#2613,.F.);
#3692=EDGE_CURVE('',#2938,#2895,#2614,.F.);
#3693=EDGE_CURVE('',#2895,#2939,#2615,.F.);
#3694=EDGE_CURVE('',#2943,#2924,#2616,.F.);
#3695=EDGE_CURVE('',#2925,#2943,#2617,.F.);
#3696=EDGE_CURVE('',#2943,#2942,#1854,.T.);
#3697=EDGE_CURVE('',#2915,#2943,#254,.T.);
#3698=EDGE_CURVE('',#2942,#2916,#255,.T.);
#3699=EDGE_CURVE('',#2944,#2945,#2618,.F.);
#3700=EDGE_CURVE('',#2946,#2944,#2619,.F.);
#3701=EDGE_CURVE('',#2945,#2946,#2620,.F.);
#3702=EDGE_CURVE('',#2947,#2948,#2621,.F.);
#3703=EDGE_CURVE('',#2949,#2947,#2622,.F.);
#3704=EDGE_CURVE('',#2948,#2949,#2623,.F.);
#3705=EDGE_CURVE('',#2950,#2951,#2624,.F.);
#3706=EDGE_CURVE('',#2952,#2950,#2625,.F.);
#3707=EDGE_CURVE('',#2951,#2952,#2626,.F.);
#3708=EDGE_CURVE('',#2945,#2952,#1855,.T.);
#3709=EDGE_CURVE('',#2950,#2944,#1856,.T.);
#3710=EDGE_CURVE('',#2907,#2951,#256,.T.);
#3711=EDGE_CURVE('',#2952,#2908,#257,.T.);
#3712=EDGE_CURVE('',#2953,#2954,#2627,.F.);
#3713=EDGE_CURVE('',#2955,#2953,#2628,.F.);
#3714=EDGE_CURVE('',#2954,#2955,#2629,.F.);
#3715=EDGE_CURVE('',#2953,#2949,#1857,.T.);
#3716=EDGE_CURVE('',#2947,#2955,#1858,.T.);
#3717=EDGE_CURVE('',#2951,#2954,#258,.T.);
#3718=EDGE_CURVE('',#2955,#2950,#259,.T.);
#3719=EDGE_CURVE('',#2905,#2953,#260,.T.);
#3720=EDGE_CURVE('',#2954,#2906,#261,.T.);
#3721=EDGE_CURVE('',#2903,#2948,#262,.T.);
#3722=EDGE_CURVE('',#2949,#2904,#263,.T.);
#3723=EDGE_CURVE('',#2948,#2946,#264,.T.);
#3724=EDGE_CURVE('',#2944,#2947,#265,.T.);
#3725=EDGE_CURVE('',#2901,#2945,#266,.T.);
#3726=EDGE_CURVE('',#2946,#2902,#267,.T.);
#3727=EDGE_CURVE('',#2956,#2957,#268,.T.);
#3728=EDGE_CURVE('',#2957,#2958,#1859,.T.);
#3729=EDGE_CURVE('',#2958,#2959,#269,.T.);
#3730=EDGE_CURVE('',#2960,#2959,#270,.T.);
#3731=EDGE_CURVE('',#2960,#2961,#271,.T.);
#3732=EDGE_CURVE('',#2961,#2962,#1860,.T.);
#3733=EDGE_CURVE('',#2962,#2963,#272,.T.);
#3734=EDGE_CURVE('',#2956,#2963,#273,.T.);
#3735=EDGE_CURVE('',#2964,#2964,#2630,.T.);
#3736=EDGE_CURVE('',#2965,#2965,#2631,.T.);
#3737=EDGE_CURVE('',#2966,#2966,#2632,.T.);
#3738=EDGE_CURVE('',#2967,#2967,#2633,.T.);
#3739=EDGE_CURVE('',#2967,#2968,#1861,.T.);
#3740=EDGE_CURVE('',#2968,#2968,#2634,.T.);
#3741=EDGE_CURVE('',#2969,#2969,#2635,.T.);
#3742=EDGE_CURVE('',#2969,#2965,#1862,.T.);
#3743=EDGE_CURVE('',#2970,#2970,#2636,.T.);
#3744=EDGE_CURVE('',#2970,#2964,#1863,.T.);
#3745=EDGE_CURVE('',#2971,#2971,#2637,.T.);
#3746=EDGE_CURVE('',#2971,#2972,#1864,.T.);
#3747=EDGE_CURVE('',#2972,#2972,#2638,.T.);
#3748=EDGE_CURVE('',#2973,#2974,#1865,.T.);
#3749=EDGE_CURVE('',#2973,#2975,#1866,.T.);
#3750=EDGE_CURVE('',#2975,#2976,#1867,.T.);
#3751=EDGE_CURVE('',#2974,#2976,#1868,.T.);
#3752=EDGE_CURVE('',#2977,#2973,#1869,.T.);
#3753=EDGE_CURVE('',#2977,#2978,#1870,.T.);
#3754=EDGE_CURVE('',#2978,#2975,#1871,.T.);
#3755=EDGE_CURVE('',#2979,#2977,#1872,.T.);
#3756=EDGE_CURVE('',#2979,#2980,#1873,.T.);
#3757=EDGE_CURVE('',#2980,#2978,#1874,.T.);
#3758=EDGE_CURVE('',#2981,#2979,#1875,.T.);
#3759=EDGE_CURVE('',#2981,#2982,#1876,.T.);
#3760=EDGE_CURVE('',#2982,#2980,#1877,.T.);
#3761=EDGE_CURVE('',#2983,#2981,#1878,.T.);
#3762=EDGE_CURVE('',#2983,#2984,#1879,.T.);
#3763=EDGE_CURVE('',#2984,#2982,#1880,.T.);
#3764=EDGE_CURVE('',#2974,#2983,#1881,.T.);
#3765=EDGE_CURVE('',#2976,#2984,#1882,.T.);
#3766=EDGE_CURVE('',#2985,#2985,#2639,.T.);
#3767=EDGE_CURVE('',#2986,#2987,#1883,.T.);
#3768=EDGE_CURVE('',#2986,#2988,#1884,.T.);
#3769=EDGE_CURVE('',#2988,#2989,#1885,.T.);
#3770=EDGE_CURVE('',#2987,#2989,#1886,.T.);
#3771=EDGE_CURVE('',#2990,#2986,#1887,.T.);
#3772=EDGE_CURVE('',#2990,#2991,#1888,.T.);
#3773=EDGE_CURVE('',#2991,#2988,#1889,.T.);
#3774=EDGE_CURVE('',#2992,#2990,#1890,.T.);
#3775=EDGE_CURVE('',#2992,#2993,#1891,.T.);
#3776=EDGE_CURVE('',#2993,#2991,#1892,.T.);
#3777=EDGE_CURVE('',#2994,#2992,#1893,.T.);
#3778=EDGE_CURVE('',#2994,#2995,#1894,.T.);
#3779=EDGE_CURVE('',#2995,#2993,#1895,.T.);
#3780=EDGE_CURVE('',#2996,#2994,#1896,.T.);
#3781=EDGE_CURVE('',#2996,#2997,#1897,.T.);
#3782=EDGE_CURVE('',#2997,#2995,#1898,.T.);
#3783=EDGE_CURVE('',#2987,#2996,#1899,.T.);
#3784=EDGE_CURVE('',#2989,#2997,#1900,.T.);
#3785=EDGE_CURVE('',#2998,#2998,#2640,.T.);
#3786=EDGE_CURVE('',#2998,#2999,#1901,.T.);
#3787=EDGE_CURVE('',#2999,#2999,#2641,.T.);
#3788=EDGE_CURVE('',#2985,#3000,#1902,.T.);
#3789=EDGE_CURVE('',#3000,#3000,#2642,.T.);
#3790=EDGE_CURVE('',#3001,#3002,#1903,.T.);
#3791=EDGE_CURVE('',#3003,#3001,#1904,.T.);
#3792=EDGE_CURVE('',#3004,#3003,#1905,.T.);
#3793=EDGE_CURVE('',#3004,#3002,#1906,.T.);
#3794=EDGE_CURVE('',#3005,#3006,#1907,.T.);
#3795=EDGE_CURVE('',#3005,#3007,#1908,.T.);
#3796=EDGE_CURVE('',#3008,#3007,#1909,.T.);
#3797=EDGE_CURVE('',#3006,#3008,#1910,.T.);
#3798=EDGE_CURVE('',#3009,#3010,#1911,.T.);
#3799=EDGE_CURVE('',#3009,#3011,#1912,.T.);
#3800=EDGE_CURVE('',#3012,#3011,#1913,.T.);
#3801=EDGE_CURVE('',#3010,#3012,#1914,.T.);
#3802=EDGE_CURVE('',#3013,#3014,#1915,.T.);
#3803=EDGE_CURVE('',#3013,#3015,#1916,.T.);
#3804=EDGE_CURVE('',#3016,#3015,#1917,.T.);
#3805=EDGE_CURVE('',#3014,#3016,#1918,.T.);
#3806=EDGE_CURVE('',#3017,#3018,#1919,.T.);
#3807=EDGE_CURVE('',#3017,#3019,#1920,.T.);
#3808=EDGE_CURVE('',#3020,#3019,#1921,.T.);
#3809=EDGE_CURVE('',#3018,#3020,#1922,.T.);
#3810=EDGE_CURVE('',#3021,#3022,#1923,.T.);
#3811=EDGE_CURVE('',#3023,#3021,#1924,.T.);
#3812=EDGE_CURVE('',#3024,#3023,#1925,.T.);
#3813=EDGE_CURVE('',#3024,#3022,#1926,.T.);
#3814=EDGE_CURVE('',#3025,#3026,#1927,.T.);
#3815=EDGE_CURVE('',#3027,#3025,#1928,.T.);
#3816=EDGE_CURVE('',#3028,#3027,#1929,.T.);
#3817=EDGE_CURVE('',#3028,#3026,#1930,.T.);
#3818=EDGE_CURVE('',#3029,#3029,#2643,.T.);
#3819=EDGE_CURVE('',#3030,#3030,#2644,.T.);
#3820=EDGE_CURVE('',#3002,#3017,#1931,.T.);
#3821=EDGE_CURVE('',#3019,#3004,#1932,.T.);
#3822=EDGE_CURVE('',#3022,#3005,#1933,.T.);
#3823=EDGE_CURVE('',#3007,#3024,#1934,.T.);
#3824=EDGE_CURVE('',#3026,#3009,#1935,.T.);
#3825=EDGE_CURVE('',#3011,#3028,#1936,.T.);
#3826=EDGE_CURVE('',#3031,#3013,#1937,.T.);
#3827=EDGE_CURVE('',#3032,#3031,#1938,.T.);
#3828=EDGE_CURVE('',#3015,#3032,#1939,.T.);
#3829=EDGE_CURVE('',#3033,#3031,#1940,.T.);
#3830=EDGE_CURVE('',#3034,#3033,#1941,.T.);
#3831=EDGE_CURVE('',#3032,#3034,#1942,.T.);
#3832=EDGE_CURVE('',#3035,#3036,#1943,.T.);
#3833=EDGE_CURVE('',#3037,#3036,#274,.T.);
#3834=EDGE_CURVE('',#3038,#3037,#275,.T.);
#3835=EDGE_CURVE('',#3039,#3038,#1944,.T.);
#3836=EDGE_CURVE('',#3040,#3039,#276,.T.);
#3837=EDGE_CURVE('',#3035,#3040,#277,.T.);
#3838=EDGE_CURVE('',#3034,#3041,#1945,.T.);
#3839=EDGE_CURVE('',#3042,#3041,#278,.T.);
#3840=EDGE_CURVE('',#3043,#3042,#279,.T.);
#3841=EDGE_CURVE('',#3044,#3043,#1946,.T.);
#3842=EDGE_CURVE('',#3045,#3044,#280,.T.);
#3843=EDGE_CURVE('',#3046,#3045,#281,.T.);
#3844=EDGE_CURVE('',#3046,#3016,#1947,.T.);
#3845=EDGE_CURVE('',#3027,#3047,#1948,.T.);
#3846=EDGE_CURVE('',#3048,#3047,#282,.T.);
#3847=EDGE_CURVE('',#3049,#3048,#283,.T.);
#3848=EDGE_CURVE('',#3050,#3049,#1949,.T.);
#3849=EDGE_CURVE('',#3051,#3050,#284,.T.);
#3850=EDGE_CURVE('',#3052,#3051,#285,.T.);
#3851=EDGE_CURVE('',#3052,#3012,#1950,.T.);
#3852=EDGE_CURVE('',#3023,#3053,#1951,.T.);
#3853=EDGE_CURVE('',#3054,#3053,#286,.T.);
#3854=EDGE_CURVE('',#2962,#3054,#287,.T.);
#3855=EDGE_CURVE('',#3055,#2961,#288,.T.);
#3856=EDGE_CURVE('',#3056,#3055,#289,.T.);
#3857=EDGE_CURVE('',#3056,#3008,#1952,.T.);
#3858=EDGE_CURVE('',#3057,#3018,#1953,.T.);
#3859=EDGE_CURVE('',#3057,#3058,#290,.T.);
#3860=EDGE_CURVE('',#3058,#3059,#1954,.T.);
#3861=EDGE_CURVE('',#3059,#3060,#291,.T.);
#3862=EDGE_CURVE('',#3001,#3060,#1955,.T.);
#3863=EDGE_CURVE('',#3046,#3036,#292,.T.);
#3864=EDGE_CURVE('',#3035,#3041,#293,.T.);
#3865=EDGE_CURVE('',#3061,#3033,#1956,.T.);
#3866=EDGE_CURVE('',#3061,#3047,#294,.T.);
#3867=EDGE_CURVE('',#3062,#3025,#1957,.T.);
#3868=EDGE_CURVE('',#3062,#3053,#295,.T.);
#3869=EDGE_CURVE('',#3063,#3021,#1958,.T.);
#3870=EDGE_CURVE('',#3063,#3064,#296,.T.);
#3871=EDGE_CURVE('',#3064,#3057,#297,.T.);
#3872=EDGE_CURVE('',#3020,#3065,#1959,.T.);
#3873=EDGE_CURVE('',#3066,#3065,#298,.T.);
#3874=EDGE_CURVE('',#3066,#3067,#299,.T.);
#3875=EDGE_CURVE('',#3068,#3067,#300,.T.);
#3876=EDGE_CURVE('',#3068,#3069,#1960,.T.);
#3877=EDGE_CURVE('',#3070,#3069,#301,.T.);
#3878=EDGE_CURVE('',#3070,#3071,#302,.T.);
#3879=EDGE_CURVE('',#3072,#3071,#303,.T.);
#3880=EDGE_CURVE('',#3072,#3003,#1961,.T.);
#3881=EDGE_CURVE('',#3060,#3073,#304,.T.);
#3882=EDGE_CURVE('',#3073,#3074,#305,.T.);
#3883=EDGE_CURVE('',#3006,#3074,#1962,.T.);
#3884=EDGE_CURVE('',#3056,#3075,#306,.T.);
#3885=EDGE_CURVE('',#3010,#3075,#1963,.T.);
#3886=EDGE_CURVE('',#3052,#3076,#307,.T.);
#3887=EDGE_CURVE('',#3014,#3076,#1964,.T.);
#3888=EDGE_CURVE('',#3077,#3078,#308,.T.);
#3889=EDGE_CURVE('',#3078,#3079,#309,.T.);
#3890=EDGE_CURVE('',#3079,#3080,#1965,.T.);
#3891=EDGE_CURVE('',#3080,#3081,#310,.T.);
#3892=EDGE_CURVE('',#3081,#3082,#311,.T.);
#3893=EDGE_CURVE('',#3077,#3082,#1966,.T.);
#3894=EDGE_CURVE('',#3083,#3083,#2645,.T.);
#3895=EDGE_CURVE('',#3083,#3030,#1967,.T.);
#3896=EDGE_CURVE('',#2966,#3029,#1968,.T.);
#3897=EDGE_CURVE('',#3077,#3084,#312,.T.);
#3898=EDGE_CURVE('',#3085,#3082,#313,.T.);
#3899=EDGE_CURVE('',#3086,#3085,#314,.T.);
#3900=EDGE_CURVE('',#3087,#3086,#1969,.T.);
#3901=EDGE_CURVE('',#3084,#3087,#315,.T.);
#3902=EDGE_CURVE('',#3045,#3037,#316,.T.);
#3903=EDGE_CURVE('',#3084,#3088,#317,.T.);
#3904=EDGE_CURVE('',#3088,#3078,#318,.T.);
#3905=EDGE_CURVE('',#3038,#3044,#319,.T.);
#3906=EDGE_CURVE('',#3089,#3087,#320,.T.);
#3907=EDGE_CURVE('',#3088,#3089,#2646,.F.);
#3908=EDGE_CURVE('',#3043,#3039,#321,.T.);
#3909=EDGE_CURVE('',#3086,#3090,#322,.T.);
#3910=EDGE_CURVE('',#3090,#3089,#1970,.T.);
#3911=EDGE_CURVE('',#3040,#3042,#323,.T.);
#3912=EDGE_CURVE('',#3081,#3091,#324,.T.);
#3913=EDGE_CURVE('',#3091,#3085,#325,.T.);
#3914=EDGE_CURVE('',#3092,#3076,#326,.T.);
#3915=EDGE_CURVE('',#3093,#3092,#327,.T.);
#3916=EDGE_CURVE('',#3094,#3093,#1971,.T.);
#3917=EDGE_CURVE('',#3095,#3094,#328,.T.);
#3918=EDGE_CURVE('',#3061,#3095,#329,.T.);
#3919=EDGE_CURVE('',#3051,#3092,#330,.T.);
#3920=EDGE_CURVE('',#3093,#3050,#331,.T.);
#3921=EDGE_CURVE('',#3049,#3094,#332,.T.);
#3922=EDGE_CURVE('',#3095,#3048,#333,.T.);
#3923=EDGE_CURVE('',#3096,#3075,#334,.T.);
#3924=EDGE_CURVE('',#2958,#3096,#335,.T.);
#3925=EDGE_CURVE('',#3097,#2957,#336,.T.);
#3926=EDGE_CURVE('',#3062,#3097,#337,.T.);
#3927=EDGE_CURVE('',#3055,#3096,#338,.T.);
#3928=EDGE_CURVE('',#3097,#3054,#339,.T.);
#3929=EDGE_CURVE('',#3098,#3074,#340,.T.);
#3930=EDGE_CURVE('',#3099,#3098,#341,.T.);
#3931=EDGE_CURVE('',#3100,#3099,#1972,.T.);
#3932=EDGE_CURVE('',#3101,#3100,#342,.T.);
#3933=EDGE_CURVE('',#3063,#3101,#343,.T.);
#3934=EDGE_CURVE('',#3073,#3102,#344,.T.);
#3935=EDGE_CURVE('',#3102,#3098,#345,.T.);
#3936=EDGE_CURVE('',#3103,#3102,#2647,.F.);
#3937=EDGE_CURVE('',#3099,#3103,#346,.T.);
#3938=EDGE_CURVE('',#3103,#3104,#1973,.T.);
#3939=EDGE_CURVE('',#3104,#3100,#347,.T.);
#3940=EDGE_CURVE('',#3101,#3105,#348,.T.);
#3941=EDGE_CURVE('',#3105,#3064,#349,.T.);
#3942=EDGE_CURVE('',#3105,#3104,#2648,.F.);
#3943=EDGE_CURVE('',#3104,#3058,#2649,.F.);
#3944=EDGE_CURVE('',#3058,#3105,#2650,.F.);
#3945=EDGE_CURVE('',#3090,#3091,#2651,.F.);
#3946=EDGE_CURVE('',#3091,#3106,#2652,.F.);
#3947=EDGE_CURVE('',#3106,#3090,#2653,.F.);
#3948=EDGE_CURVE('',#3102,#3059,#2654,.F.);
#3949=EDGE_CURVE('',#3059,#3103,#2655,.F.);
#3950=EDGE_CURVE('',#3107,#3088,#2656,.F.);
#3951=EDGE_CURVE('',#3089,#3107,#2657,.F.);
#3952=EDGE_CURVE('',#3107,#3106,#1974,.T.);
#3953=EDGE_CURVE('',#3079,#3107,#350,.T.);
#3954=EDGE_CURVE('',#3106,#3080,#351,.T.);
#3955=EDGE_CURVE('',#3108,#3109,#2658,.F.);
#3956=EDGE_CURVE('',#3110,#3108,#2659,.F.);
#3957=EDGE_CURVE('',#3109,#3110,#2660,.F.);
#3958=EDGE_CURVE('',#3111,#3112,#2661,.F.);
#3959=EDGE_CURVE('',#3113,#3111,#2662,.F.);
#3960=EDGE_CURVE('',#3112,#3113,#2663,.F.);
#3961=EDGE_CURVE('',#3114,#3115,#2664,.F.);
#3962=EDGE_CURVE('',#3116,#3114,#2665,.F.);
#3963=EDGE_CURVE('',#3115,#3116,#2666,.F.);
#3964=EDGE_CURVE('',#3109,#3116,#1975,.T.);
#3965=EDGE_CURVE('',#3114,#3108,#1976,.T.);
#3966=EDGE_CURVE('',#3071,#3115,#352,.T.);
#3967=EDGE_CURVE('',#3116,#3072,#353,.T.);
#3968=EDGE_CURVE('',#3117,#3118,#2667,.F.);
#3969=EDGE_CURVE('',#3119,#3117,#2668,.F.);
#3970=EDGE_CURVE('',#3118,#3119,#2669,.F.);
#3971=EDGE_CURVE('',#3117,#3113,#1977,.T.);
#3972=EDGE_CURVE('',#3111,#3119,#1978,.T.);
#3973=EDGE_CURVE('',#3115,#3118,#354,.T.);
#3974=EDGE_CURVE('',#3119,#3114,#355,.T.);
#3975=EDGE_CURVE('',#3069,#3117,#356,.T.);
#3976=EDGE_CURVE('',#3118,#3070,#357,.T.);
#3977=EDGE_CURVE('',#3067,#3112,#358,.T.);
#3978=EDGE_CURVE('',#3113,#3068,#359,.T.);
#3979=EDGE_CURVE('',#3112,#3110,#360,.T.);
#3980=EDGE_CURVE('',#3108,#3111,#361,.T.);
#3981=EDGE_CURVE('',#3065,#3109,#362,.T.);
#3982=EDGE_CURVE('',#3110,#3066,#363,.T.);
#3983=EDGE_CURVE('',#3120,#3120,#2670,.T.);
#3984=EDGE_CURVE('',#3120,#3121,#1979,.T.);
#3985=EDGE_CURVE('',#3121,#3121,#2671,.T.);
#3986=EDGE_CURVE('',#3122,#3122,#2672,.T.);
#3987=EDGE_CURVE('',#3122,#3123,#1980,.T.);
#3988=EDGE_CURVE('',#3123,#3123,#2673,.T.);
#3989=EDGE_CURVE('',#3124,#3124,#2674,.T.);
#3990=EDGE_CURVE('',#3125,#3125,#2675,.T.);
#3991=EDGE_CURVE('',#3126,#3126,#2676,.T.);
#3992=EDGE_CURVE('',#3126,#3124,#1981,.T.);
#3993=EDGE_CURVE('',#3127,#3127,#2677,.T.);
#3994=EDGE_CURVE('',#3128,#3128,#2678,.T.);
#3995=EDGE_CURVE('',#3129,#3129,#2679,.T.);
#3996=EDGE_CURVE('',#3129,#3127,#1982,.T.);
#3997=EDGE_CURVE('',#3130,#3130,#2680,.T.);
#3998=EDGE_CURVE('',#3131,#3131,#2681,.T.);
#3999=EDGE_CURVE('',#3132,#3132,#2682,.T.);
#4000=EDGE_CURVE('',#3132,#3130,#1983,.T.);
#4001=EDGE_CURVE('',#3133,#3133,#2683,.T.);
#4002=EDGE_CURVE('',#3134,#3134,#2684,.T.);
#4003=EDGE_CURVE('',#3135,#3135,#2685,.T.);
#4004=EDGE_CURVE('',#3135,#3133,#1984,.T.);
#4005=EDGE_CURVE('',#3125,#3136,#1985,.T.);
#4006=EDGE_CURVE('',#3136,#3136,#2686,.T.);
#4007=EDGE_CURVE('',#3128,#3137,#1986,.T.);
#4008=EDGE_CURVE('',#3137,#3137,#2687,.T.);
#4009=EDGE_CURVE('',#3131,#3138,#1987,.T.);
#4010=EDGE_CURVE('',#3138,#3138,#2688,.T.);
#4011=EDGE_CURVE('',#3134,#3139,#1988,.T.);
#4012=EDGE_CURVE('',#3139,#3139,#2689,.T.);
#4013=EDGE_CURVE('',#3140,#3141,#2690,.T.);
#4014=EDGE_CURVE('',#3141,#3142,#364,.T.);
#4015=EDGE_CURVE('',#3142,#3143,#2691,.T.);
#4016=EDGE_CURVE('',#3143,#3140,#365,.T.);
#4017=EDGE_CURVE('',#3144,#3145,#2692,.T.);
#4018=EDGE_CURVE('',#3145,#3141,#1989,.T.);
#4019=EDGE_CURVE('',#3140,#3144,#1990,.T.);
#4020=EDGE_CURVE('',#3146,#3147,#2693,.T.);
#4021=EDGE_CURVE('',#3147,#3145,#366,.T.);
#4022=EDGE_CURVE('',#3144,#3146,#367,.T.);
#4023=EDGE_CURVE('',#3148,#3149,#2694,.T.);
#4024=EDGE_CURVE('',#3149,#3147,#368,.T.);
#4025=EDGE_CURVE('',#3146,#3148,#369,.T.);
#4026=EDGE_CURVE('',#3150,#3151,#2695,.T.);
#4027=EDGE_CURVE('',#3151,#3149,#370,.T.);
#4028=EDGE_CURVE('',#3148,#3150,#371,.T.);
#4029=EDGE_CURVE('',#3152,#3153,#2696,.T.);
#4030=EDGE_CURVE('',#3153,#3151,#1991,.T.);
#4031=EDGE_CURVE('',#3150,#3152,#1992,.T.);
#4032=EDGE_CURVE('',#3154,#3155,#2697,.T.);
#4033=EDGE_CURVE('',#3155,#3153,#372,.T.);
#4034=EDGE_CURVE('',#3152,#3154,#373,.T.);
#4035=EDGE_CURVE('',#3142,#3155,#374,.T.);
#4036=EDGE_CURVE('',#3154,#3143,#375,.T.);
#4037=EDGE_CURVE('',#3156,#3153,#376,.T.);
#4038=EDGE_CURVE('',#3157,#3156,#1993,.T.);
#4039=EDGE_CURVE('',#3151,#3157,#377,.T.);
#4040=EDGE_CURVE('',#3155,#3158,#378,.T.);
#4041=EDGE_CURVE('',#3158,#3156,#379,.T.);
#4042=EDGE_CURVE('',#3159,#3142,#380,.T.);
#4043=EDGE_CURVE('',#3158,#3159,#381,.T.);
#4044=EDGE_CURVE('',#3141,#3160,#382,.T.);
#4045=EDGE_CURVE('',#3160,#3159,#383,.T.);
#4046=EDGE_CURVE('',#3161,#3145,#384,.T.);
#4047=EDGE_CURVE('',#3160,#3161,#1994,.T.);
#4048=EDGE_CURVE('',#3157,#3162,#385,.T.);
#4049=EDGE_CURVE('',#3162,#3149,#386,.T.);
#4050=EDGE_CURVE('',#3147,#3163,#387,.T.);
#4051=EDGE_CURVE('',#3163,#3161,#388,.T.);
#4052=EDGE_CURVE('',#3163,#3162,#389,.T.);
#4053=EDGE_CURVE('',#3164,#3165,#1995,.T.);
#4054=EDGE_CURVE('',#3164,#3166,#390,.T.);
#4055=EDGE_CURVE('',#3166,#3167,#2698,.F.);
#4056=EDGE_CURVE('',#3167,#3165,#391,.T.);
#4057=EDGE_CURVE('',#3168,#3169,#1996,.T.);
#4058=EDGE_CURVE('',#3168,#3164,#392,.T.);
#4059=EDGE_CURVE('',#3165,#3169,#393,.T.);
#4060=EDGE_CURVE('',#3170,#3171,#1997,.T.);
#4061=EDGE_CURVE('',#3170,#3168,#394,.T.);
#4062=EDGE_CURVE('',#3169,#3171,#395,.T.);
#4063=EDGE_CURVE('',#3172,#3173,#1998,.T.);
#4064=EDGE_CURVE('',#3172,#3170,#396,.T.);
#4065=EDGE_CURVE('',#3171,#3173,#397,.T.);
#4066=EDGE_CURVE('',#3174,#3175,#1999,.T.);
#4067=EDGE_CURVE('',#3174,#3172,#398,.T.);
#4068=EDGE_CURVE('',#3173,#3175,#399,.T.);
#4069=EDGE_CURVE('',#3176,#3177,#2000,.T.);
#4070=EDGE_CURVE('',#3176,#3174,#400,.T.);
#4071=EDGE_CURVE('',#3175,#3177,#401,.T.);
#4072=EDGE_CURVE('',#3178,#3179,#2001,.T.);
#4073=EDGE_CURVE('',#3178,#3176,#402,.T.);
#4074=EDGE_CURVE('',#3177,#3179,#403,.T.);
#4075=EDGE_CURVE('',#3180,#3181,#2002,.T.);
#4076=EDGE_CURVE('',#3180,#3178,#404,.T.);
#4077=EDGE_CURVE('',#3179,#3181,#405,.T.);
#4078=EDGE_CURVE('',#3182,#3183,#2003,.T.);
#4079=EDGE_CURVE('',#3182,#3180,#406,.T.);
#4080=EDGE_CURVE('',#3181,#3183,#407,.T.);
#4081=EDGE_CURVE('',#3184,#3185,#2004,.T.);
#4082=EDGE_CURVE('',#3184,#3182,#408,.T.);
#4083=EDGE_CURVE('',#3183,#3185,#409,.T.);
#4084=EDGE_CURVE('',#3186,#3187,#2005,.T.);
#4085=EDGE_CURVE('',#3186,#3184,#410,.T.);
#4086=EDGE_CURVE('',#3185,#3187,#411,.T.);
#4087=EDGE_CURVE('',#3188,#3189,#2006,.T.);
#4088=EDGE_CURVE('',#3188,#3186,#412,.T.);
#4089=EDGE_CURVE('',#3187,#3189,#413,.T.);
#4090=EDGE_CURVE('',#3190,#3191,#2007,.T.);
#4091=EDGE_CURVE('',#3190,#3188,#414,.T.);
#4092=EDGE_CURVE('',#3189,#3191,#415,.T.);
#4093=EDGE_CURVE('',#3192,#3193,#2008,.T.);
#4094=EDGE_CURVE('',#3192,#3190,#416,.T.);
#4095=EDGE_CURVE('',#3191,#3193,#417,.T.);
#4096=EDGE_CURVE('',#3194,#3195,#2009,.T.);
#4097=EDGE_CURVE('',#3194,#3192,#418,.T.);
#4098=EDGE_CURVE('',#3193,#3195,#419,.T.);
#4099=EDGE_CURVE('',#3196,#3197,#2010,.T.);
#4100=EDGE_CURVE('',#3196,#3194,#420,.T.);
#4101=EDGE_CURVE('',#3195,#3197,#421,.T.);
#4102=EDGE_CURVE('',#3198,#3199,#2011,.T.);
#4103=EDGE_CURVE('',#3198,#3196,#422,.T.);
#4104=EDGE_CURVE('',#3197,#3199,#423,.T.);
#4105=EDGE_CURVE('',#3200,#3201,#2012,.T.);
#4106=EDGE_CURVE('',#3200,#3198,#424,.T.);
#4107=EDGE_CURVE('',#3199,#3201,#425,.T.);
#4108=EDGE_CURVE('',#3202,#3203,#2013,.T.);
#4109=EDGE_CURVE('',#3202,#3200,#426,.T.);
#4110=EDGE_CURVE('',#3201,#3203,#427,.T.);
#4111=EDGE_CURVE('',#3204,#3205,#2014,.T.);
#4112=EDGE_CURVE('',#3204,#3202,#428,.T.);
#4113=EDGE_CURVE('',#3203,#3205,#429,.T.);
#4114=EDGE_CURVE('',#3206,#3207,#2015,.T.);
#4115=EDGE_CURVE('',#3206,#3204,#430,.T.);
#4116=EDGE_CURVE('',#3205,#3207,#431,.T.);
#4117=EDGE_CURVE('',#3208,#3209,#2016,.T.);
#4118=EDGE_CURVE('',#3208,#3206,#432,.T.);
#4119=EDGE_CURVE('',#3207,#3209,#433,.T.);
#4120=EDGE_CURVE('',#3210,#3211,#2017,.T.);
#4121=EDGE_CURVE('',#3210,#3208,#434,.T.);
#4122=EDGE_CURVE('',#3209,#3211,#435,.T.);
#4123=EDGE_CURVE('',#3212,#3213,#2018,.T.);
#4124=EDGE_CURVE('',#3212,#3210,#436,.T.);
#4125=EDGE_CURVE('',#3211,#3213,#437,.T.);
#4126=EDGE_CURVE('',#3214,#3215,#2019,.T.);
#4127=EDGE_CURVE('',#3214,#3212,#438,.T.);
#4128=EDGE_CURVE('',#3213,#3215,#439,.T.);
#4129=EDGE_CURVE('',#3216,#3217,#2020,.T.);
#4130=EDGE_CURVE('',#3216,#3214,#440,.T.);
#4131=EDGE_CURVE('',#3215,#3217,#441,.T.);
#4132=EDGE_CURVE('',#3218,#3219,#2021,.T.);
#4133=EDGE_CURVE('',#3218,#3216,#442,.T.);
#4134=EDGE_CURVE('',#3217,#3219,#443,.T.);
#4135=EDGE_CURVE('',#3220,#3221,#2022,.T.);
#4136=EDGE_CURVE('',#3220,#3218,#444,.T.);
#4137=EDGE_CURVE('',#3219,#3221,#445,.T.);
#4138=EDGE_CURVE('',#3222,#3223,#2023,.T.);
#4139=EDGE_CURVE('',#3222,#3220,#446,.T.);
#4140=EDGE_CURVE('',#3221,#3223,#447,.T.);
#4141=EDGE_CURVE('',#3224,#3225,#2024,.T.);
#4142=EDGE_CURVE('',#3224,#3222,#448,.T.);
#4143=EDGE_CURVE('',#3223,#3225,#449,.T.);
#4144=EDGE_CURVE('',#3226,#3227,#2025,.T.);
#4145=EDGE_CURVE('',#3226,#3228,#450,.T.);
#4146=EDGE_CURVE('',#3228,#3229,#2699,.T.);
#4147=EDGE_CURVE('',#3227,#3229,#451,.T.);
#4148=EDGE_CURVE('',#3230,#3231,#2026,.T.);
#4149=EDGE_CURVE('',#3230,#3226,#452,.T.);
#4150=EDGE_CURVE('',#3231,#3227,#453,.T.);
#4151=EDGE_CURVE('',#3232,#3233,#2027,.T.);
#4152=EDGE_CURVE('',#3232,#3230,#454,.T.);
#4153=EDGE_CURVE('',#3233,#3231,#455,.T.);
#4154=EDGE_CURVE('',#3234,#3235,#2028,.T.);
#4155=EDGE_CURVE('',#3234,#3232,#456,.T.);
#4156=EDGE_CURVE('',#3235,#3233,#457,.T.);
#4157=EDGE_CURVE('',#3236,#3237,#2029,.T.);
#4158=EDGE_CURVE('',#3236,#3234,#458,.T.);
#4159=EDGE_CURVE('',#3237,#3235,#459,.T.);
#4160=EDGE_CURVE('',#3238,#3239,#2030,.T.);
#4161=EDGE_CURVE('',#3238,#3236,#460,.T.);
#4162=EDGE_CURVE('',#3239,#3237,#461,.T.);
#4163=EDGE_CURVE('',#3240,#3241,#2031,.T.);
#4164=EDGE_CURVE('',#3240,#3238,#462,.T.);
#4165=EDGE_CURVE('',#3241,#3239,#463,.T.);
#4166=EDGE_CURVE('',#3242,#3243,#2032,.T.);
#4167=EDGE_CURVE('',#3242,#3240,#464,.T.);
#4168=EDGE_CURVE('',#3243,#3241,#465,.T.);
#4169=EDGE_CURVE('',#3244,#3245,#2033,.T.);
#4170=EDGE_CURVE('',#3244,#3242,#466,.T.);
#4171=EDGE_CURVE('',#3245,#3243,#467,.T.);
#4172=EDGE_CURVE('',#3246,#3247,#2034,.T.);
#4173=EDGE_CURVE('',#3246,#3244,#468,.T.);
#4174=EDGE_CURVE('',#3247,#3245,#469,.T.);
#4175=EDGE_CURVE('',#3248,#3249,#2035,.T.);
#4176=EDGE_CURVE('',#3248,#3246,#470,.T.);
#4177=EDGE_CURVE('',#3249,#3247,#471,.T.);
#4178=EDGE_CURVE('',#3250,#3251,#2036,.T.);
#4179=EDGE_CURVE('',#3250,#3248,#472,.T.);
#4180=EDGE_CURVE('',#3251,#3249,#473,.T.);
#4181=EDGE_CURVE('',#3252,#3253,#2037,.T.);
#4182=EDGE_CURVE('',#3252,#3250,#474,.T.);
#4183=EDGE_CURVE('',#3253,#3251,#475,.T.);
#4184=EDGE_CURVE('',#3254,#3255,#2038,.T.);
#4185=EDGE_CURVE('',#3254,#3252,#476,.T.);
#4186=EDGE_CURVE('',#3255,#3253,#477,.T.);
#4187=EDGE_CURVE('',#3256,#3257,#2039,.T.);
#4188=EDGE_CURVE('',#3256,#3254,#478,.T.);
#4189=EDGE_CURVE('',#3257,#3255,#479,.T.);
#4190=EDGE_CURVE('',#3258,#3259,#2040,.T.);
#4191=EDGE_CURVE('',#3258,#3256,#480,.T.);
#4192=EDGE_CURVE('',#3259,#3257,#481,.T.);
#4193=EDGE_CURVE('',#3260,#3261,#2041,.T.);
#4194=EDGE_CURVE('',#3260,#3258,#482,.T.);
#4195=EDGE_CURVE('',#3261,#3259,#483,.T.);
#4196=EDGE_CURVE('',#3262,#3263,#2042,.T.);
#4197=EDGE_CURVE('',#3262,#3260,#484,.T.);
#4198=EDGE_CURVE('',#3263,#3261,#485,.T.);
#4199=EDGE_CURVE('',#3264,#3265,#2043,.T.);
#4200=EDGE_CURVE('',#3264,#3262,#486,.T.);
#4201=EDGE_CURVE('',#3265,#3263,#487,.T.);
#4202=EDGE_CURVE('',#3266,#3267,#2044,.T.);
#4203=EDGE_CURVE('',#3266,#3264,#488,.T.);
#4204=EDGE_CURVE('',#3267,#3265,#489,.T.);
#4205=EDGE_CURVE('',#3268,#3269,#2045,.T.);
#4206=EDGE_CURVE('',#3268,#3266,#490,.T.);
#4207=EDGE_CURVE('',#3269,#3267,#491,.T.);
#4208=EDGE_CURVE('',#3270,#3271,#2046,.T.);
#4209=EDGE_CURVE('',#3270,#3268,#492,.T.);
#4210=EDGE_CURVE('',#3271,#3269,#493,.T.);
#4211=EDGE_CURVE('',#3272,#3273,#2047,.T.);
#4212=EDGE_CURVE('',#3272,#3270,#494,.T.);
#4213=EDGE_CURVE('',#3273,#3271,#495,.T.);
#4214=EDGE_CURVE('',#3274,#3275,#2048,.T.);
#4215=EDGE_CURVE('',#3274,#3272,#496,.T.);
#4216=EDGE_CURVE('',#3275,#3273,#497,.T.);
#4217=EDGE_CURVE('',#3276,#3277,#2049,.T.);
#4218=EDGE_CURVE('',#3276,#3274,#498,.T.);
#4219=EDGE_CURVE('',#3277,#3275,#499,.T.);
#4220=EDGE_CURVE('',#3278,#3279,#2050,.T.);
#4221=EDGE_CURVE('',#3278,#3276,#500,.T.);
#4222=EDGE_CURVE('',#3279,#3277,#501,.T.);
#4223=EDGE_CURVE('',#3280,#3281,#2051,.T.);
#4224=EDGE_CURVE('',#3280,#3278,#502,.T.);
#4225=EDGE_CURVE('',#3281,#3279,#503,.T.);
#4226=EDGE_CURVE('',#3282,#3283,#2052,.T.);
#4227=EDGE_CURVE('',#3282,#3280,#504,.T.);
#4228=EDGE_CURVE('',#3283,#3281,#505,.T.);
#4229=EDGE_CURVE('',#3284,#3285,#2053,.T.);
#4230=EDGE_CURVE('',#3284,#3282,#506,.T.);
#4231=EDGE_CURVE('',#3285,#3283,#507,.T.);
#4232=EDGE_CURVE('',#3286,#3287,#2054,.T.);
#4233=EDGE_CURVE('',#3286,#3284,#508,.T.);
#4234=EDGE_CURVE('',#3287,#3285,#509,.T.);
#4235=EDGE_CURVE('',#3229,#3288,#510,.T.);
#4236=EDGE_CURVE('',#3289,#3228,#511,.T.);
#4237=EDGE_CURVE('',#3290,#3289,#2700,.T.);
#4238=EDGE_CURVE('',#3288,#3290,#512,.T.);
#4239=EDGE_CURVE('',#3288,#3291,#2055,.T.);
#4240=EDGE_CURVE('',#3291,#3291,#2701,.T.);
#4241=EDGE_CURVE('',#3292,#3286,#513,.T.);
#4242=EDGE_CURVE('',#3166,#3292,#514,.T.);
#4243=EDGE_CURVE('',#3289,#3224,#515,.T.);
#4244=EDGE_CURVE('',#3293,#3287,#516,.T.);
#4245=EDGE_CURVE('',#3292,#3293,#2702,.T.);
#4246=EDGE_CURVE('',#3225,#3290,#517,.T.);
#4247=EDGE_CURVE('',#3293,#3167,#518,.T.);
#4248=EDGE_CURVE('',#3294,#3295,#2056,.T.);
#4249=EDGE_CURVE('',#3294,#3296,#2057,.T.);
#4250=EDGE_CURVE('',#3296,#3297,#2058,.T.);
#4251=EDGE_CURVE('',#3295,#3297,#2059,.T.);
#4252=EDGE_CURVE('',#3298,#3294,#2060,.T.);
#4253=EDGE_CURVE('',#3298,#3299,#2061,.T.);
#4254=EDGE_CURVE('',#3299,#3296,#2062,.T.);
#4255=EDGE_CURVE('',#3300,#3298,#2063,.T.);
#4256=EDGE_CURVE('',#3300,#3301,#2064,.T.);
#4257=EDGE_CURVE('',#3301,#3299,#2065,.T.);
#4258=EDGE_CURVE('',#3302,#3300,#2066,.T.);
#4259=EDGE_CURVE('',#3302,#3303,#2067,.T.);
#4260=EDGE_CURVE('',#3303,#3301,#2068,.T.);
#4261=EDGE_CURVE('',#3304,#3302,#2069,.T.);
#4262=EDGE_CURVE('',#3304,#3305,#2070,.T.);
#4263=EDGE_CURVE('',#3305,#3303,#2071,.T.);
#4264=EDGE_CURVE('',#3295,#3304,#2072,.T.);
#4265=EDGE_CURVE('',#3297,#3305,#2073,.T.);
#4266=EDGE_CURVE('',#3306,#3306,#2703,.T.);
#4267=EDGE_CURVE('',#3306,#3307,#2074,.T.);
#4268=EDGE_CURVE('',#3307,#3307,#2704,.T.);
#4269=EDGE_CURVE('',#3308,#3309,#2075,.T.);
#4270=EDGE_CURVE('',#3310,#3309,#2705,.F.);
#4271=EDGE_CURVE('',#3310,#3308,#519,.T.);
#4272=EDGE_CURVE('',#3311,#3312,#2076,.T.);
#4273=EDGE_CURVE('',#3312,#3313,#520,.T.);
#4274=EDGE_CURVE('',#3309,#3313,#2706,.F.);
#4275=EDGE_CURVE('',#3308,#3311,#521,.T.);
#4276=EDGE_CURVE('',#3314,#3315,#2077,.T.);
#4277=EDGE_CURVE('',#3315,#3312,#522,.T.);
#4278=EDGE_CURVE('',#3311,#3314,#523,.T.);
#4279=EDGE_CURVE('',#3316,#3317,#2078,.T.);
#4280=EDGE_CURVE('',#3317,#3315,#524,.T.);
#4281=EDGE_CURVE('',#3314,#3316,#525,.T.);
#4282=EDGE_CURVE('',#3318,#3319,#2079,.T.);
#4283=EDGE_CURVE('',#3318,#3320,#526,.T.);
#4284=EDGE_CURVE('',#3321,#3320,#2707,.T.);
#4285=EDGE_CURVE('',#3321,#3319,#527,.T.);
#4286=EDGE_CURVE('',#3322,#3323,#2080,.T.);
#4287=EDGE_CURVE('',#3323,#3324,#528,.T.);
#4288=EDGE_CURVE('',#3325,#3324,#2708,.T.);
#4289=EDGE_CURVE('',#3322,#3325,#529,.T.);
#4290=EDGE_CURVE('',#3326,#3327,#2081,.T.);
#4291=EDGE_CURVE('',#3327,#3323,#530,.T.);
#4292=EDGE_CURVE('',#3326,#3322,#531,.T.);
#4293=EDGE_CURVE('',#3328,#3329,#2082,.T.);
#4294=EDGE_CURVE('',#3329,#3327,#532,.T.);
#4295=EDGE_CURVE('',#3328,#3326,#533,.T.);
#4296=EDGE_CURVE('',#3330,#3331,#2083,.T.);
#4297=EDGE_CURVE('',#3331,#3329,#534,.T.);
#4298=EDGE_CURVE('',#3330,#3328,#535,.T.);
#4299=EDGE_CURVE('',#3332,#3333,#2084,.T.);
#4300=EDGE_CURVE('',#3334,#3332,#536,.T.);
#4301=EDGE_CURVE('',#3335,#3334,#2709,.T.);
#4302=EDGE_CURVE('',#3335,#3333,#537,.T.);
#4303=EDGE_CURVE('',#3333,#3331,#538,.T.);
#4304=EDGE_CURVE('',#3332,#3330,#539,.T.);
#4305=EDGE_CURVE('',#3324,#3310,#540,.T.);
#4306=EDGE_CURVE('',#3320,#3335,#541,.T.);
#4307=EDGE_CURVE('',#3316,#3318,#542,.T.);
#4308=EDGE_CURVE('',#3313,#3325,#543,.T.);
#4309=EDGE_CURVE('',#3319,#3317,#544,.T.);
#4310=EDGE_CURVE('',#3334,#3321,#545,.T.);
#4311=EDGE_CURVE('',#3336,#3337,#2085,.T.);
#4312=EDGE_CURVE('',#3337,#3338,#2086,.T.);
#4313=EDGE_CURVE('',#3338,#3339,#2087,.T.);
#4314=EDGE_CURVE('',#3339,#3340,#2088,.T.);
#4315=EDGE_CURVE('',#3340,#3341,#2089,.T.);
#4316=EDGE_CURVE('',#3341,#3336,#2090,.T.);
#4317=EDGE_CURVE('',#3342,#3343,#2091,.T.);
#4318=EDGE_CURVE('',#3343,#3336,#2092,.T.);
#4319=EDGE_CURVE('',#3342,#3341,#2093,.T.);
#4320=EDGE_CURVE('',#3344,#3342,#2094,.T.);
#4321=EDGE_CURVE('',#3344,#3340,#2095,.T.);
#4322=EDGE_CURVE('',#3345,#3344,#2096,.T.);
#4323=EDGE_CURVE('',#3345,#3339,#2097,.T.);
#4324=EDGE_CURVE('',#3346,#3345,#2098,.T.);
#4325=EDGE_CURVE('',#3346,#3338,#2099,.T.);
#4326=EDGE_CURVE('',#3347,#3346,#2100,.T.);
#4327=EDGE_CURVE('',#3347,#3337,#2101,.T.);
#4328=EDGE_CURVE('',#3343,#3347,#2102,.T.);
#4329=EDGE_CURVE('',#3348,#3348,#2710,.T.);
#4330=EDGE_CURVE('',#3348,#3349,#2103,.T.);
#4331=EDGE_CURVE('',#3349,#3349,#2711,.T.);
#4332=EDGE_CURVE('',#3350,#3350,#2712,.T.);
#4333=EDGE_CURVE('',#3350,#3351,#2104,.T.);
#4334=EDGE_CURVE('',#3351,#3351,#2713,.T.);
#4335=ORIENTED_EDGE('',*,*,#3352,.F.);
#4336=ORIENTED_EDGE('',*,*,#3353,.T.);
#4337=ORIENTED_EDGE('',*,*,#3354,.F.);
#4338=ORIENTED_EDGE('',*,*,#3353,.F.);
#4339=ORIENTED_EDGE('',*,*,#3355,.F.);
#4340=ORIENTED_EDGE('',*,*,#3356,.T.);
#4341=ORIENTED_EDGE('',*,*,#3357,.F.);
#4342=ORIENTED_EDGE('',*,*,#3356,.F.);
#4343=ORIENTED_EDGE('',*,*,#3358,.F.);
#4344=ORIENTED_EDGE('',*,*,#3359,.T.);
#4345=ORIENTED_EDGE('',*,*,#3360,.F.);
#4346=ORIENTED_EDGE('',*,*,#3359,.F.);
#4347=ORIENTED_EDGE('',*,*,#3361,.F.);
#4348=ORIENTED_EDGE('',*,*,#3362,.F.);
#4349=ORIENTED_EDGE('',*,*,#3363,.F.);
#4350=ORIENTED_EDGE('',*,*,#3364,.F.);
#4351=ORIENTED_EDGE('',*,*,#3365,.F.);
#4352=ORIENTED_EDGE('',*,*,#3362,.T.);
#4353=ORIENTED_EDGE('',*,*,#3366,.T.);
#4354=ORIENTED_EDGE('',*,*,#3367,.F.);
#4355=ORIENTED_EDGE('',*,*,#3368,.F.);
#4356=ORIENTED_EDGE('',*,*,#3364,.T.);
#4357=ORIENTED_EDGE('',*,*,#3361,.T.);
#4358=ORIENTED_EDGE('',*,*,#3369,.F.);
#4359=ORIENTED_EDGE('',*,*,#3370,.T.);
#4360=ORIENTED_EDGE('',*,*,#3371,.F.);
#4361=ORIENTED_EDGE('',*,*,#3372,.F.);
#4362=ORIENTED_EDGE('',*,*,#3373,.F.);
#4363=ORIENTED_EDGE('',*,*,#3374,.T.);
#4364=ORIENTED_EDGE('',*,*,#3375,.F.);
#4365=ORIENTED_EDGE('',*,*,#3376,.F.);
#4366=ORIENTED_EDGE('',*,*,#3374,.F.);
#4367=ORIENTED_EDGE('',*,*,#3377,.F.);
#4368=ORIENTED_EDGE('',*,*,#3366,.F.);
#4369=ORIENTED_EDGE('',*,*,#3376,.T.);
#4370=ORIENTED_EDGE('',*,*,#3378,.F.);
#4371=ORIENTED_EDGE('',*,*,#3379,.F.);
#4372=ORIENTED_EDGE('',*,*,#3380,.F.);
#4373=ORIENTED_EDGE('',*,*,#3377,.T.);
#4374=ORIENTED_EDGE('',*,*,#3379,.T.);
#4375=ORIENTED_EDGE('',*,*,#3378,.T.);
#4376=ORIENTED_EDGE('',*,*,#3375,.T.);
#4377=ORIENTED_EDGE('',*,*,#3373,.T.);
#4378=ORIENTED_EDGE('',*,*,#3381,.T.);
#4379=ORIENTED_EDGE('',*,*,#3382,.T.);
#4380=ORIENTED_EDGE('',*,*,#3383,.T.);
#4381=ORIENTED_EDGE('',*,*,#3384,.T.);
#4382=ORIENTED_EDGE('',*,*,#3385,.T.);
#4383=ORIENTED_EDGE('',*,*,#3386,.T.);
#4384=ORIENTED_EDGE('',*,*,#3387,.T.);
#4385=ORIENTED_EDGE('',*,*,#3388,.T.);
#4386=ORIENTED_EDGE('',*,*,#3389,.T.);
#4387=ORIENTED_EDGE('',*,*,#3390,.T.);
#4388=ORIENTED_EDGE('',*,*,#3391,.T.);
#4389=ORIENTED_EDGE('',*,*,#3392,.T.);
#4390=ORIENTED_EDGE('',*,*,#3393,.T.);
#4391=ORIENTED_EDGE('',*,*,#3352,.T.);
#4392=ORIENTED_EDGE('',*,*,#3355,.T.);
#4393=ORIENTED_EDGE('',*,*,#3358,.T.);
#4394=ORIENTED_EDGE('',*,*,#3394,.F.);
#4395=ORIENTED_EDGE('',*,*,#3395,.T.);
#4396=ORIENTED_EDGE('',*,*,#3396,.F.);
#4397=ORIENTED_EDGE('',*,*,#3370,.F.);
#4398=ORIENTED_EDGE('',*,*,#3368,.T.);
#4399=ORIENTED_EDGE('',*,*,#3397,.T.);
#4400=ORIENTED_EDGE('',*,*,#3398,.T.);
#4401=ORIENTED_EDGE('',*,*,#3399,.T.);
#4402=ORIENTED_EDGE('',*,*,#3400,.T.);
#4403=ORIENTED_EDGE('',*,*,#3394,.T.);
#4404=ORIENTED_EDGE('',*,*,#3369,.T.);
#4405=ORIENTED_EDGE('',*,*,#3363,.T.);
#4406=ORIENTED_EDGE('',*,*,#3365,.T.);
#4407=ORIENTED_EDGE('',*,*,#3367,.T.);
#4408=ORIENTED_EDGE('',*,*,#3380,.T.);
#4409=ORIENTED_EDGE('',*,*,#3393,.F.);
#4410=ORIENTED_EDGE('',*,*,#3401,.F.);
#4411=ORIENTED_EDGE('',*,*,#3397,.F.);
#4412=ORIENTED_EDGE('',*,*,#3402,.F.);
#4413=ORIENTED_EDGE('',*,*,#3403,.F.);
#4414=ORIENTED_EDGE('',*,*,#3404,.T.);
#4415=ORIENTED_EDGE('',*,*,#3389,.F.);
#4416=ORIENTED_EDGE('',*,*,#3401,.T.);
#4417=ORIENTED_EDGE('',*,*,#3392,.F.);
#4418=ORIENTED_EDGE('',*,*,#3405,.F.);
#4419=ORIENTED_EDGE('',*,*,#3398,.F.);
#4420=ORIENTED_EDGE('',*,*,#3405,.T.);
#4421=ORIENTED_EDGE('',*,*,#3391,.F.);
#4422=ORIENTED_EDGE('',*,*,#3406,.F.);
#4423=ORIENTED_EDGE('',*,*,#3399,.F.);
#4424=ORIENTED_EDGE('',*,*,#3406,.T.);
#4425=ORIENTED_EDGE('',*,*,#3390,.F.);
#4426=ORIENTED_EDGE('',*,*,#3404,.F.);
#4427=ORIENTED_EDGE('',*,*,#3407,.F.);
#4428=ORIENTED_EDGE('',*,*,#3395,.F.);
#4429=ORIENTED_EDGE('',*,*,#3400,.F.);
#4430=ORIENTED_EDGE('',*,*,#3396,.T.);
#4431=ORIENTED_EDGE('',*,*,#3407,.T.);
#4432=ORIENTED_EDGE('',*,*,#3403,.T.);
#4433=ORIENTED_EDGE('',*,*,#3408,.F.);
#4434=ORIENTED_EDGE('',*,*,#3409,.F.);
#4435=ORIENTED_EDGE('',*,*,#3410,.F.);
#4436=ORIENTED_EDGE('',*,*,#3411,.F.);
#4437=ORIENTED_EDGE('',*,*,#3412,.F.);
#4438=ORIENTED_EDGE('',*,*,#3413,.F.);
#4439=ORIENTED_EDGE('',*,*,#3414,.F.);
#4440=ORIENTED_EDGE('',*,*,#3415,.F.);
#4441=ORIENTED_EDGE('',*,*,#3371,.T.);
#4442=ORIENTED_EDGE('',*,*,#3354,.T.);
#4443=ORIENTED_EDGE('',*,*,#3357,.T.);
#4444=ORIENTED_EDGE('',*,*,#3360,.T.);
#4445=ORIENTED_EDGE('',*,*,#3402,.T.);
#4446=ORIENTED_EDGE('',*,*,#3388,.F.);
#4447=ORIENTED_EDGE('',*,*,#3416,.T.);
#4448=ORIENTED_EDGE('',*,*,#3408,.T.);
#4449=ORIENTED_EDGE('',*,*,#3417,.F.);
#4450=ORIENTED_EDGE('',*,*,#3414,.T.);
#4451=ORIENTED_EDGE('',*,*,#3418,.T.);
#4452=ORIENTED_EDGE('',*,*,#3382,.F.);
#4453=ORIENTED_EDGE('',*,*,#3416,.F.);
#4454=ORIENTED_EDGE('',*,*,#3387,.F.);
#4455=ORIENTED_EDGE('',*,*,#3419,.F.);
#4456=ORIENTED_EDGE('',*,*,#3409,.T.);
#4457=ORIENTED_EDGE('',*,*,#3410,.T.);
#4458=ORIENTED_EDGE('',*,*,#3419,.T.);
#4459=ORIENTED_EDGE('',*,*,#3386,.F.);
#4460=ORIENTED_EDGE('',*,*,#3420,.F.);
#4461=ORIENTED_EDGE('',*,*,#3411,.T.);
#4462=ORIENTED_EDGE('',*,*,#3420,.T.);
#4463=ORIENTED_EDGE('',*,*,#3385,.F.);
#4464=ORIENTED_EDGE('',*,*,#3421,.F.);
#4465=ORIENTED_EDGE('',*,*,#3412,.T.);
#4466=ORIENTED_EDGE('',*,*,#3421,.T.);
#4467=ORIENTED_EDGE('',*,*,#3384,.F.);
#4468=ORIENTED_EDGE('',*,*,#3422,.F.);
#4469=ORIENTED_EDGE('',*,*,#3413,.T.);
#4470=ORIENTED_EDGE('',*,*,#3422,.T.);
#4471=ORIENTED_EDGE('',*,*,#3383,.F.);
#4472=ORIENTED_EDGE('',*,*,#3418,.F.);
#4473=ORIENTED_EDGE('',*,*,#3372,.T.);
#4474=ORIENTED_EDGE('',*,*,#3415,.T.);
#4475=ORIENTED_EDGE('',*,*,#3417,.T.);
#4476=ORIENTED_EDGE('',*,*,#3381,.F.);
#4477=ORIENTED_EDGE('',*,*,#3423,.F.);
#4478=ORIENTED_EDGE('',*,*,#3424,.T.);
#4479=ORIENTED_EDGE('',*,*,#3425,.F.);
#4480=ORIENTED_EDGE('',*,*,#3424,.F.);
#4481=ORIENTED_EDGE('',*,*,#3426,.F.);
#4482=ORIENTED_EDGE('',*,*,#3427,.T.);
#4483=ORIENTED_EDGE('',*,*,#3428,.F.);
#4484=ORIENTED_EDGE('',*,*,#3427,.F.);
#4485=ORIENTED_EDGE('',*,*,#3429,.F.);
#4486=ORIENTED_EDGE('',*,*,#3430,.T.);
#4487=ORIENTED_EDGE('',*,*,#3431,.F.);
#4488=ORIENTED_EDGE('',*,*,#3430,.F.);
#4489=ORIENTED_EDGE('',*,*,#3432,.F.);
#4490=ORIENTED_EDGE('',*,*,#3433,.T.);
#4491=ORIENTED_EDGE('',*,*,#3434,.F.);
#4492=ORIENTED_EDGE('',*,*,#3435,.F.);
#4493=ORIENTED_EDGE('',*,*,#3436,.T.);
#4494=ORIENTED_EDGE('',*,*,#3432,.T.);
#4495=ORIENTED_EDGE('',*,*,#3437,.T.);
#4496=ORIENTED_EDGE('',*,*,#3438,.T.);
#4497=ORIENTED_EDGE('',*,*,#3439,.T.);
#4498=ORIENTED_EDGE('',*,*,#3440,.F.);
#4499=ORIENTED_EDGE('',*,*,#3441,.F.);
#4500=ORIENTED_EDGE('',*,*,#3442,.F.);
#4501=ORIENTED_EDGE('',*,*,#3437,.F.);
#4502=ORIENTED_EDGE('',*,*,#3435,.T.);
#4503=ORIENTED_EDGE('',*,*,#3443,.F.);
#4504=ORIENTED_EDGE('',*,*,#3444,.F.);
#4505=ORIENTED_EDGE('',*,*,#3445,.F.);
#4506=ORIENTED_EDGE('',*,*,#3446,.T.);
#4507=ORIENTED_EDGE('',*,*,#3447,.F.);
#4508=ORIENTED_EDGE('',*,*,#3442,.T.);
#4509=ORIENTED_EDGE('',*,*,#3448,.F.);
#4510=ORIENTED_EDGE('',*,*,#3449,.F.);
#4511=ORIENTED_EDGE('',*,*,#3438,.F.);
#4512=ORIENTED_EDGE('',*,*,#3449,.T.);
#4513=ORIENTED_EDGE('',*,*,#3450,.F.);
#4514=ORIENTED_EDGE('',*,*,#3451,.F.);
#4515=ORIENTED_EDGE('',*,*,#3439,.F.);
#4516=ORIENTED_EDGE('',*,*,#3451,.T.);
#4517=ORIENTED_EDGE('',*,*,#3452,.F.);
#4518=ORIENTED_EDGE('',*,*,#3446,.F.);
#4519=ORIENTED_EDGE('',*,*,#3453,.F.);
#4520=ORIENTED_EDGE('',*,*,#3433,.F.);
#4521=ORIENTED_EDGE('',*,*,#3436,.F.);
#4522=ORIENTED_EDGE('',*,*,#3434,.T.);
#4523=ORIENTED_EDGE('',*,*,#3453,.T.);
#4524=ORIENTED_EDGE('',*,*,#3445,.T.);
#4525=ORIENTED_EDGE('',*,*,#3454,.F.);
#4526=ORIENTED_EDGE('',*,*,#3455,.F.);
#4527=ORIENTED_EDGE('',*,*,#3456,.F.);
#4528=ORIENTED_EDGE('',*,*,#3457,.F.);
#4529=ORIENTED_EDGE('',*,*,#3458,.F.);
#4530=ORIENTED_EDGE('',*,*,#3459,.F.);
#4531=ORIENTED_EDGE('',*,*,#3460,.F.);
#4532=ORIENTED_EDGE('',*,*,#3461,.F.);
#4533=ORIENTED_EDGE('',*,*,#3443,.T.);
#4534=ORIENTED_EDGE('',*,*,#3425,.T.);
#4535=ORIENTED_EDGE('',*,*,#3428,.T.);
#4536=ORIENTED_EDGE('',*,*,#3431,.T.);
#4537=ORIENTED_EDGE('',*,*,#3444,.T.);
#4538=ORIENTED_EDGE('',*,*,#3462,.F.);
#4539=ORIENTED_EDGE('',*,*,#3463,.T.);
#4540=ORIENTED_EDGE('',*,*,#3454,.T.);
#4541=ORIENTED_EDGE('',*,*,#3464,.F.);
#4542=ORIENTED_EDGE('',*,*,#3460,.T.);
#4543=ORIENTED_EDGE('',*,*,#3465,.T.);
#4544=ORIENTED_EDGE('',*,*,#3466,.F.);
#4545=ORIENTED_EDGE('',*,*,#3463,.F.);
#4546=ORIENTED_EDGE('',*,*,#3467,.F.);
#4547=ORIENTED_EDGE('',*,*,#3468,.F.);
#4548=ORIENTED_EDGE('',*,*,#3455,.T.);
#4549=ORIENTED_EDGE('',*,*,#3456,.T.);
#4550=ORIENTED_EDGE('',*,*,#3468,.T.);
#4551=ORIENTED_EDGE('',*,*,#3469,.F.);
#4552=ORIENTED_EDGE('',*,*,#3470,.F.);
#4553=ORIENTED_EDGE('',*,*,#3457,.T.);
#4554=ORIENTED_EDGE('',*,*,#3470,.T.);
#4555=ORIENTED_EDGE('',*,*,#3471,.F.);
#4556=ORIENTED_EDGE('',*,*,#3472,.F.);
#4557=ORIENTED_EDGE('',*,*,#3458,.T.);
#4558=ORIENTED_EDGE('',*,*,#3472,.T.);
#4559=ORIENTED_EDGE('',*,*,#3473,.F.);
#4560=ORIENTED_EDGE('',*,*,#3474,.F.);
#4561=ORIENTED_EDGE('',*,*,#3459,.T.);
#4562=ORIENTED_EDGE('',*,*,#3474,.T.);
#4563=ORIENTED_EDGE('',*,*,#3475,.F.);
#4564=ORIENTED_EDGE('',*,*,#3465,.F.);
#4565=ORIENTED_EDGE('',*,*,#3476,.T.);
#4566=ORIENTED_EDGE('',*,*,#3466,.T.);
#4567=ORIENTED_EDGE('',*,*,#3475,.T.);
#4568=ORIENTED_EDGE('',*,*,#3473,.T.);
#4569=ORIENTED_EDGE('',*,*,#3471,.T.);
#4570=ORIENTED_EDGE('',*,*,#3469,.T.);
#4571=ORIENTED_EDGE('',*,*,#3467,.T.);
#4572=ORIENTED_EDGE('',*,*,#3462,.T.);
#4573=ORIENTED_EDGE('',*,*,#3447,.T.);
#4574=ORIENTED_EDGE('',*,*,#3452,.T.);
#4575=ORIENTED_EDGE('',*,*,#3450,.T.);
#4576=ORIENTED_EDGE('',*,*,#3448,.T.);
#4577=ORIENTED_EDGE('',*,*,#3441,.T.);
#4578=ORIENTED_EDGE('',*,*,#3423,.T.);
#4579=ORIENTED_EDGE('',*,*,#3426,.T.);
#4580=ORIENTED_EDGE('',*,*,#3429,.T.);
#4581=ORIENTED_EDGE('',*,*,#3440,.T.);
#4582=ORIENTED_EDGE('',*,*,#3461,.T.);
#4583=ORIENTED_EDGE('',*,*,#3464,.T.);
#4584=ORIENTED_EDGE('',*,*,#3476,.F.);
#4585=ORIENTED_EDGE('',*,*,#3477,.T.);
#4586=ORIENTED_EDGE('',*,*,#3478,.T.);
#4587=ORIENTED_EDGE('',*,*,#3479,.F.);
#4588=ORIENTED_EDGE('',*,*,#3478,.F.);
#4589=ORIENTED_EDGE('',*,*,#3480,.F.);
#4590=ORIENTED_EDGE('',*,*,#3477,.F.);
#4591=ORIENTED_EDGE('',*,*,#3481,.F.);
#4592=ORIENTED_EDGE('',*,*,#3479,.T.);
#4593=ORIENTED_EDGE('',*,*,#3482,.F.);
#4594=ORIENTED_EDGE('',*,*,#3483,.T.);
#4595=ORIENTED_EDGE('',*,*,#3481,.T.);
#4596=ORIENTED_EDGE('',*,*,#3483,.F.);
#4597=ORIENTED_EDGE('',*,*,#3484,.T.);
#4598=ORIENTED_EDGE('',*,*,#3485,.F.);
#4599=ORIENTED_EDGE('',*,*,#3484,.F.);
#4600=ORIENTED_EDGE('',*,*,#3486,.T.);
#4601=ORIENTED_EDGE('',*,*,#3487,.T.);
#4602=ORIENTED_EDGE('',*,*,#3486,.F.);
#4603=ORIENTED_EDGE('',*,*,#3487,.F.);
#4604=ORIENTED_EDGE('',*,*,#3480,.T.);
#4605=ORIENTED_EDGE('',*,*,#3488,.T.);
#4606=ORIENTED_EDGE('',*,*,#3485,.T.);
#4607=ORIENTED_EDGE('',*,*,#3488,.F.);
#4608=ORIENTED_EDGE('',*,*,#3482,.T.);
#4609=ORIENTED_EDGE('',*,*,#3489,.F.);
#4610=ORIENTED_EDGE('',*,*,#3490,.F.);
#4611=ORIENTED_EDGE('',*,*,#3491,.F.);
#4612=ORIENTED_EDGE('',*,*,#3492,.F.);
#4613=ORIENTED_EDGE('',*,*,#3493,.F.);
#4614=ORIENTED_EDGE('',*,*,#3494,.F.);
#4615=ORIENTED_EDGE('',*,*,#3495,.F.);
#4616=ORIENTED_EDGE('',*,*,#3496,.F.);
#4617=ORIENTED_EDGE('',*,*,#3496,.T.);
#4618=ORIENTED_EDGE('',*,*,#3497,.F.);
#4619=ORIENTED_EDGE('',*,*,#3490,.T.);
#4620=ORIENTED_EDGE('',*,*,#3498,.F.);
#4621=ORIENTED_EDGE('',*,*,#3493,.T.);
#4622=ORIENTED_EDGE('',*,*,#3498,.T.);
#4623=ORIENTED_EDGE('',*,*,#3489,.T.);
#4624=ORIENTED_EDGE('',*,*,#3499,.F.);
#4625=ORIENTED_EDGE('',*,*,#3495,.T.);
#4626=ORIENTED_EDGE('',*,*,#3500,.F.);
#4627=ORIENTED_EDGE('',*,*,#3491,.T.);
#4628=ORIENTED_EDGE('',*,*,#3497,.T.);
#4629=ORIENTED_EDGE('',*,*,#3494,.T.);
#4630=ORIENTED_EDGE('',*,*,#3499,.T.);
#4631=ORIENTED_EDGE('',*,*,#3492,.T.);
#4632=ORIENTED_EDGE('',*,*,#3500,.T.);
#4633=ORIENTED_EDGE('',*,*,#3501,.T.);
#4634=ORIENTED_EDGE('',*,*,#3502,.T.);
#4635=ORIENTED_EDGE('',*,*,#3503,.T.);
#4636=ORIENTED_EDGE('',*,*,#3504,.F.);
#4637=ORIENTED_EDGE('',*,*,#3505,.T.);
#4638=ORIENTED_EDGE('',*,*,#3506,.T.);
#4639=ORIENTED_EDGE('',*,*,#3507,.T.);
#4640=ORIENTED_EDGE('',*,*,#3508,.F.);
#4641=ORIENTED_EDGE('',*,*,#3509,.T.);
#4642=ORIENTED_EDGE('',*,*,#3510,.T.);
#4643=ORIENTED_EDGE('',*,*,#3511,.T.);
#4644=ORIENTED_EDGE('',*,*,#3512,.F.);
#4645=ORIENTED_EDGE('',*,*,#3513,.T.);
#4646=ORIENTED_EDGE('',*,*,#3514,.F.);
#4647=ORIENTED_EDGE('',*,*,#3513,.F.);
#4648=ORIENTED_EDGE('',*,*,#3515,.F.);
#4649=ORIENTED_EDGE('',*,*,#3516,.T.);
#4650=ORIENTED_EDGE('',*,*,#3510,.F.);
#4651=ORIENTED_EDGE('',*,*,#3516,.F.);
#4652=ORIENTED_EDGE('',*,*,#3517,.F.);
#4653=ORIENTED_EDGE('',*,*,#3518,.T.);
#4654=ORIENTED_EDGE('',*,*,#3509,.F.);
#4655=ORIENTED_EDGE('',*,*,#3518,.F.);
#4656=ORIENTED_EDGE('',*,*,#3519,.F.);
#4657=ORIENTED_EDGE('',*,*,#3520,.T.);
#4658=ORIENTED_EDGE('',*,*,#3521,.F.);
#4659=ORIENTED_EDGE('',*,*,#3520,.F.);
#4660=ORIENTED_EDGE('',*,*,#3522,.F.);
#4661=ORIENTED_EDGE('',*,*,#3523,.T.);
#4662=ORIENTED_EDGE('',*,*,#3524,.T.);
#4663=ORIENTED_EDGE('',*,*,#3523,.F.);
#4664=ORIENTED_EDGE('',*,*,#3524,.F.);
#4665=ORIENTED_EDGE('',*,*,#3525,.F.);
#4666=ORIENTED_EDGE('',*,*,#3526,.F.);
#4667=ORIENTED_EDGE('',*,*,#3527,.T.);
#4668=ORIENTED_EDGE('',*,*,#3528,.T.);
#4669=ORIENTED_EDGE('',*,*,#3527,.F.);
#4670=ORIENTED_EDGE('',*,*,#3528,.F.);
#4671=ORIENTED_EDGE('',*,*,#3529,.F.);
#4672=ORIENTED_EDGE('',*,*,#3525,.T.);
#4673=ORIENTED_EDGE('',*,*,#3530,.T.);
#4674=ORIENTED_EDGE('',*,*,#3531,.F.);
#4675=ORIENTED_EDGE('',*,*,#3530,.F.);
#4676=ORIENTED_EDGE('',*,*,#3529,.T.);
#4677=ORIENTED_EDGE('',*,*,#3532,.T.);
#4678=ORIENTED_EDGE('',*,*,#3533,.F.);
#4679=ORIENTED_EDGE('',*,*,#3532,.F.);
#4680=ORIENTED_EDGE('',*,*,#3534,.F.);
#4681=ORIENTED_EDGE('',*,*,#3535,.F.);
#4682=ORIENTED_EDGE('',*,*,#3536,.F.);
#4683=ORIENTED_EDGE('',*,*,#3537,.T.);
#4684=ORIENTED_EDGE('',*,*,#3538,.F.);
#4685=ORIENTED_EDGE('',*,*,#3539,.T.);
#4686=ORIENTED_EDGE('',*,*,#3540,.F.);
#4687=ORIENTED_EDGE('',*,*,#3541,.F.);
#4688=ORIENTED_EDGE('',*,*,#3542,.F.);
#4689=ORIENTED_EDGE('',*,*,#3543,.T.);
#4690=ORIENTED_EDGE('',*,*,#3544,.F.);
#4691=ORIENTED_EDGE('',*,*,#3545,.F.);
#4692=ORIENTED_EDGE('',*,*,#3546,.F.);
#4693=ORIENTED_EDGE('',*,*,#3547,.T.);
#4694=ORIENTED_EDGE('',*,*,#3548,.F.);
#4695=ORIENTED_EDGE('',*,*,#3549,.F.);
#4696=ORIENTED_EDGE('',*,*,#3550,.F.);
#4697=ORIENTED_EDGE('',*,*,#3551,.T.);
#4698=ORIENTED_EDGE('',*,*,#3552,.F.);
#4699=ORIENTED_EDGE('',*,*,#3553,.F.);
#4700=ORIENTED_EDGE('',*,*,#3554,.F.);
#4701=ORIENTED_EDGE('',*,*,#3555,.F.);
#4702=ORIENTED_EDGE('',*,*,#3556,.F.);
#4703=ORIENTED_EDGE('',*,*,#3557,.T.);
#4704=ORIENTED_EDGE('',*,*,#3558,.F.);
#4705=ORIENTED_EDGE('',*,*,#3559,.F.);
#4706=ORIENTED_EDGE('',*,*,#3560,.F.);
#4707=ORIENTED_EDGE('',*,*,#3561,.T.);
#4708=ORIENTED_EDGE('',*,*,#3562,.F.);
#4709=ORIENTED_EDGE('',*,*,#3531,.T.);
#4710=ORIENTED_EDGE('',*,*,#3563,.F.);
#4711=ORIENTED_EDGE('',*,*,#3533,.T.);
#4712=ORIENTED_EDGE('',*,*,#3564,.F.);
#4713=ORIENTED_EDGE('',*,*,#3537,.F.);
#4714=ORIENTED_EDGE('',*,*,#3565,.F.);
#4715=ORIENTED_EDGE('',*,*,#3551,.F.);
#4716=ORIENTED_EDGE('',*,*,#3566,.F.);
#4717=ORIENTED_EDGE('',*,*,#3557,.F.);
#4718=ORIENTED_EDGE('',*,*,#3567,.F.);
#4719=ORIENTED_EDGE('',*,*,#3539,.F.);
#4720=ORIENTED_EDGE('',*,*,#3568,.F.);
#4721=ORIENTED_EDGE('',*,*,#3561,.F.);
#4722=ORIENTED_EDGE('',*,*,#3569,.F.);
#4723=ORIENTED_EDGE('',*,*,#3543,.F.);
#4724=ORIENTED_EDGE('',*,*,#3570,.F.);
#4725=ORIENTED_EDGE('',*,*,#3571,.F.);
#4726=ORIENTED_EDGE('',*,*,#3572,.F.);
#4727=ORIENTED_EDGE('',*,*,#3547,.F.);
#4728=ORIENTED_EDGE('',*,*,#3573,.F.);
#4729=ORIENTED_EDGE('',*,*,#3574,.F.);
#4730=ORIENTED_EDGE('',*,*,#3575,.F.);
#4731=ORIENTED_EDGE('',*,*,#3571,.T.);
#4732=ORIENTED_EDGE('',*,*,#3576,.T.);
#4733=ORIENTED_EDGE('',*,*,#3577,.F.);
#4734=ORIENTED_EDGE('',*,*,#3578,.F.);
#4735=ORIENTED_EDGE('',*,*,#3579,.F.);
#4736=ORIENTED_EDGE('',*,*,#3580,.F.);
#4737=ORIENTED_EDGE('',*,*,#3581,.F.);
#4738=ORIENTED_EDGE('',*,*,#3548,.T.);
#4739=ORIENTED_EDGE('',*,*,#3572,.T.);
#4740=ORIENTED_EDGE('',*,*,#3575,.T.);
#4741=ORIENTED_EDGE('',*,*,#3582,.T.);
#4742=ORIENTED_EDGE('',*,*,#3583,.F.);
#4743=ORIENTED_EDGE('',*,*,#3584,.F.);
#4744=ORIENTED_EDGE('',*,*,#3585,.F.);
#4745=ORIENTED_EDGE('',*,*,#3586,.F.);
#4746=ORIENTED_EDGE('',*,*,#3587,.F.);
#4747=ORIENTED_EDGE('',*,*,#3588,.T.);
#4748=ORIENTED_EDGE('',*,*,#3544,.T.);
#4749=ORIENTED_EDGE('',*,*,#3569,.T.);
#4750=ORIENTED_EDGE('',*,*,#3560,.T.);
#4751=ORIENTED_EDGE('',*,*,#3589,.T.);
#4752=ORIENTED_EDGE('',*,*,#3590,.F.);
#4753=ORIENTED_EDGE('',*,*,#3591,.F.);
#4754=ORIENTED_EDGE('',*,*,#3592,.F.);
#4755=ORIENTED_EDGE('',*,*,#3593,.F.);
#4756=ORIENTED_EDGE('',*,*,#3594,.F.);
#4757=ORIENTED_EDGE('',*,*,#3595,.T.);
#4758=ORIENTED_EDGE('',*,*,#3540,.T.);
#4759=ORIENTED_EDGE('',*,*,#3567,.T.);
#4760=ORIENTED_EDGE('',*,*,#3556,.T.);
#4761=ORIENTED_EDGE('',*,*,#3596,.T.);
#4762=ORIENTED_EDGE('',*,*,#3597,.F.);
#4763=ORIENTED_EDGE('',*,*,#3598,.F.);
#4764=ORIENTED_EDGE('',*,*,#3506,.F.);
#4765=ORIENTED_EDGE('',*,*,#3599,.F.);
#4766=ORIENTED_EDGE('',*,*,#3600,.F.);
#4767=ORIENTED_EDGE('',*,*,#3601,.T.);
#4768=ORIENTED_EDGE('',*,*,#3534,.T.);
#4769=ORIENTED_EDGE('',*,*,#3564,.T.);
#4770=ORIENTED_EDGE('',*,*,#3550,.T.);
#4771=ORIENTED_EDGE('',*,*,#3602,.F.);
#4772=ORIENTED_EDGE('',*,*,#3603,.T.);
#4773=ORIENTED_EDGE('',*,*,#3604,.T.);
#4774=ORIENTED_EDGE('',*,*,#3605,.T.);
#4775=ORIENTED_EDGE('',*,*,#3606,.F.);
#4776=ORIENTED_EDGE('',*,*,#3549,.T.);
#4777=ORIENTED_EDGE('',*,*,#3588,.F.);
#4778=ORIENTED_EDGE('',*,*,#3607,.T.);
#4779=ORIENTED_EDGE('',*,*,#3576,.F.);
#4780=ORIENTED_EDGE('',*,*,#3608,.T.);
#4781=ORIENTED_EDGE('',*,*,#3582,.F.);
#4782=ORIENTED_EDGE('',*,*,#3574,.T.);
#4783=ORIENTED_EDGE('',*,*,#3609,.F.);
#4784=ORIENTED_EDGE('',*,*,#3610,.T.);
#4785=ORIENTED_EDGE('',*,*,#3589,.F.);
#4786=ORIENTED_EDGE('',*,*,#3559,.T.);
#4787=ORIENTED_EDGE('',*,*,#3611,.F.);
#4788=ORIENTED_EDGE('',*,*,#3612,.T.);
#4789=ORIENTED_EDGE('',*,*,#3596,.F.);
#4790=ORIENTED_EDGE('',*,*,#3555,.T.);
#4791=ORIENTED_EDGE('',*,*,#3613,.F.);
#4792=ORIENTED_EDGE('',*,*,#3614,.T.);
#4793=ORIENTED_EDGE('',*,*,#3615,.T.);
#4794=ORIENTED_EDGE('',*,*,#3602,.T.);
#4795=ORIENTED_EDGE('',*,*,#3553,.T.);
#4796=ORIENTED_EDGE('',*,*,#3616,.T.);
#4797=ORIENTED_EDGE('',*,*,#3617,.F.);
#4798=ORIENTED_EDGE('',*,*,#3618,.T.);
#4799=ORIENTED_EDGE('',*,*,#3619,.F.);
#4800=ORIENTED_EDGE('',*,*,#3620,.T.);
#4801=ORIENTED_EDGE('',*,*,#3621,.F.);
#4802=ORIENTED_EDGE('',*,*,#3622,.T.);
#4803=ORIENTED_EDGE('',*,*,#3623,.F.);
#4804=ORIENTED_EDGE('',*,*,#3624,.T.);
#4805=ORIENTED_EDGE('',*,*,#3535,.T.);
#4806=ORIENTED_EDGE('',*,*,#3606,.T.);
#4807=ORIENTED_EDGE('',*,*,#3625,.T.);
#4808=ORIENTED_EDGE('',*,*,#3626,.T.);
#4809=ORIENTED_EDGE('',*,*,#3627,.F.);
#4810=ORIENTED_EDGE('',*,*,#3541,.T.);
#4811=ORIENTED_EDGE('',*,*,#3601,.F.);
#4812=ORIENTED_EDGE('',*,*,#3628,.T.);
#4813=ORIENTED_EDGE('',*,*,#3629,.F.);
#4814=ORIENTED_EDGE('',*,*,#3545,.T.);
#4815=ORIENTED_EDGE('',*,*,#3595,.F.);
#4816=ORIENTED_EDGE('',*,*,#3630,.T.);
#4817=ORIENTED_EDGE('',*,*,#3631,.F.);
#4818=ORIENTED_EDGE('',*,*,#3632,.T.);
#4819=ORIENTED_EDGE('',*,*,#3633,.T.);
#4820=ORIENTED_EDGE('',*,*,#3634,.T.);
#4821=ORIENTED_EDGE('',*,*,#3635,.T.);
#4822=ORIENTED_EDGE('',*,*,#3636,.T.);
#4823=ORIENTED_EDGE('',*,*,#3637,.F.);
#4824=ORIENTED_EDGE('',*,*,#3638,.F.);
#4825=ORIENTED_EDGE('',*,*,#3639,.T.);
#4826=ORIENTED_EDGE('',*,*,#3563,.T.);
#4827=ORIENTED_EDGE('',*,*,#3639,.F.);
#4828=ORIENTED_EDGE('',*,*,#3511,.F.);
#4829=ORIENTED_EDGE('',*,*,#3640,.T.);
#4830=ORIENTED_EDGE('',*,*,#3562,.T.);
#4831=ORIENTED_EDGE('',*,*,#3640,.F.);
#4832=ORIENTED_EDGE('',*,*,#3641,.F.);
#4833=ORIENTED_EDGE('',*,*,#3637,.T.);
#4834=ORIENTED_EDGE('',*,*,#3642,.F.);
#4835=ORIENTED_EDGE('',*,*,#3643,.F.);
#4836=ORIENTED_EDGE('',*,*,#3644,.F.);
#4837=ORIENTED_EDGE('',*,*,#3645,.F.);
#4838=ORIENTED_EDGE('',*,*,#3577,.T.);
#4839=ORIENTED_EDGE('',*,*,#3607,.F.);
#4840=ORIENTED_EDGE('',*,*,#3587,.T.);
#4841=ORIENTED_EDGE('',*,*,#3646,.T.);
#4842=ORIENTED_EDGE('',*,*,#3641,.T.);
#4843=ORIENTED_EDGE('',*,*,#3647,.T.);
#4844=ORIENTED_EDGE('',*,*,#3648,.T.);
#4845=ORIENTED_EDGE('',*,*,#3632,.F.);
#4846=ORIENTED_EDGE('',*,*,#3578,.T.);
#4847=ORIENTED_EDGE('',*,*,#3646,.F.);
#4848=ORIENTED_EDGE('',*,*,#3586,.T.);
#4849=ORIENTED_EDGE('',*,*,#3649,.F.);
#4850=ORIENTED_EDGE('',*,*,#3645,.T.);
#4851=ORIENTED_EDGE('',*,*,#3650,.F.);
#4852=ORIENTED_EDGE('',*,*,#3651,.F.);
#4853=ORIENTED_EDGE('',*,*,#3647,.F.);
#4854=ORIENTED_EDGE('',*,*,#3579,.T.);
#4855=ORIENTED_EDGE('',*,*,#3649,.T.);
#4856=ORIENTED_EDGE('',*,*,#3585,.T.);
#4857=ORIENTED_EDGE('',*,*,#3652,.T.);
#4858=ORIENTED_EDGE('',*,*,#3514,.T.);
#4859=ORIENTED_EDGE('',*,*,#3521,.T.);
#4860=ORIENTED_EDGE('',*,*,#3638,.T.);
#4861=ORIENTED_EDGE('',*,*,#3644,.T.);
#4862=ORIENTED_EDGE('',*,*,#3653,.T.);
#4863=ORIENTED_EDGE('',*,*,#3654,.T.);
#4864=ORIENTED_EDGE('',*,*,#3650,.T.);
#4865=ORIENTED_EDGE('',*,*,#3580,.T.);
#4866=ORIENTED_EDGE('',*,*,#3652,.F.);
#4867=ORIENTED_EDGE('',*,*,#3584,.T.);
#4868=ORIENTED_EDGE('',*,*,#3655,.F.);
#4869=ORIENTED_EDGE('',*,*,#3581,.T.);
#4870=ORIENTED_EDGE('',*,*,#3655,.T.);
#4871=ORIENTED_EDGE('',*,*,#3583,.T.);
#4872=ORIENTED_EDGE('',*,*,#3608,.F.);
#4873=ORIENTED_EDGE('',*,*,#3642,.T.);
#4874=ORIENTED_EDGE('',*,*,#3636,.F.);
#4875=ORIENTED_EDGE('',*,*,#3656,.T.);
#4876=ORIENTED_EDGE('',*,*,#3657,.T.);
#4877=ORIENTED_EDGE('',*,*,#3546,.T.);
#4878=ORIENTED_EDGE('',*,*,#3631,.T.);
#4879=ORIENTED_EDGE('',*,*,#3658,.F.);
#4880=ORIENTED_EDGE('',*,*,#3659,.F.);
#4881=ORIENTED_EDGE('',*,*,#3660,.F.);
#4882=ORIENTED_EDGE('',*,*,#3661,.F.);
#4883=ORIENTED_EDGE('',*,*,#3662,.F.);
#4884=ORIENTED_EDGE('',*,*,#3609,.T.);
#4885=ORIENTED_EDGE('',*,*,#3573,.T.);
#4886=ORIENTED_EDGE('',*,*,#3570,.T.);
#4887=ORIENTED_EDGE('',*,*,#3658,.T.);
#4888=ORIENTED_EDGE('',*,*,#3630,.F.);
#4889=ORIENTED_EDGE('',*,*,#3594,.T.);
#4890=ORIENTED_EDGE('',*,*,#3663,.T.);
#4891=ORIENTED_EDGE('',*,*,#3659,.T.);
#4892=ORIENTED_EDGE('',*,*,#3663,.F.);
#4893=ORIENTED_EDGE('',*,*,#3593,.T.);
#4894=ORIENTED_EDGE('',*,*,#3664,.F.);
#4895=ORIENTED_EDGE('',*,*,#3660,.T.);
#4896=ORIENTED_EDGE('',*,*,#3664,.T.);
#4897=ORIENTED_EDGE('',*,*,#3592,.T.);
#4898=ORIENTED_EDGE('',*,*,#3665,.T.);
#4899=ORIENTED_EDGE('',*,*,#3661,.T.);
#4900=ORIENTED_EDGE('',*,*,#3665,.F.);
#4901=ORIENTED_EDGE('',*,*,#3591,.T.);
#4902=ORIENTED_EDGE('',*,*,#3666,.F.);
#4903=ORIENTED_EDGE('',*,*,#3662,.T.);
#4904=ORIENTED_EDGE('',*,*,#3666,.T.);
#4905=ORIENTED_EDGE('',*,*,#3590,.T.);
#4906=ORIENTED_EDGE('',*,*,#3610,.F.);
#4907=ORIENTED_EDGE('',*,*,#3542,.T.);
#4908=ORIENTED_EDGE('',*,*,#3629,.T.);
#4909=ORIENTED_EDGE('',*,*,#3667,.F.);
#4910=ORIENTED_EDGE('',*,*,#3668,.F.);
#4911=ORIENTED_EDGE('',*,*,#3502,.F.);
#4912=ORIENTED_EDGE('',*,*,#3669,.F.);
#4913=ORIENTED_EDGE('',*,*,#3670,.F.);
#4914=ORIENTED_EDGE('',*,*,#3611,.T.);
#4915=ORIENTED_EDGE('',*,*,#3558,.T.);
#4916=ORIENTED_EDGE('',*,*,#3568,.T.);
#4917=ORIENTED_EDGE('',*,*,#3667,.T.);
#4918=ORIENTED_EDGE('',*,*,#3628,.F.);
#4919=ORIENTED_EDGE('',*,*,#3600,.T.);
#4920=ORIENTED_EDGE('',*,*,#3671,.T.);
#4921=ORIENTED_EDGE('',*,*,#3504,.T.);
#4922=ORIENTED_EDGE('',*,*,#3503,.F.);
#4923=ORIENTED_EDGE('',*,*,#3668,.T.);
#4924=ORIENTED_EDGE('',*,*,#3671,.F.);
#4925=ORIENTED_EDGE('',*,*,#3599,.T.);
#4926=ORIENTED_EDGE('',*,*,#3505,.F.);
#4927=ORIENTED_EDGE('',*,*,#3508,.T.);
#4928=ORIENTED_EDGE('',*,*,#3507,.F.);
#4929=ORIENTED_EDGE('',*,*,#3598,.T.);
#4930=ORIENTED_EDGE('',*,*,#3672,.F.);
#4931=ORIENTED_EDGE('',*,*,#3669,.T.);
#4932=ORIENTED_EDGE('',*,*,#3501,.F.);
#4933=ORIENTED_EDGE('',*,*,#3670,.T.);
#4934=ORIENTED_EDGE('',*,*,#3672,.T.);
#4935=ORIENTED_EDGE('',*,*,#3597,.T.);
#4936=ORIENTED_EDGE('',*,*,#3612,.F.);
#4937=ORIENTED_EDGE('',*,*,#3538,.T.);
#4938=ORIENTED_EDGE('',*,*,#3627,.T.);
#4939=ORIENTED_EDGE('',*,*,#3673,.F.);
#4940=ORIENTED_EDGE('',*,*,#3674,.F.);
#4941=ORIENTED_EDGE('',*,*,#3675,.F.);
#4942=ORIENTED_EDGE('',*,*,#3676,.F.);
#4943=ORIENTED_EDGE('',*,*,#3677,.F.);
#4944=ORIENTED_EDGE('',*,*,#3613,.T.);
#4945=ORIENTED_EDGE('',*,*,#3554,.T.);
#4946=ORIENTED_EDGE('',*,*,#3566,.T.);
#4947=ORIENTED_EDGE('',*,*,#3673,.T.);
#4948=ORIENTED_EDGE('',*,*,#3626,.F.);
#4949=ORIENTED_EDGE('',*,*,#3678,.T.);
#4950=ORIENTED_EDGE('',*,*,#3679,.T.);
#4951=ORIENTED_EDGE('',*,*,#3674,.T.);
#4952=ORIENTED_EDGE('',*,*,#3679,.F.);
#4953=ORIENTED_EDGE('',*,*,#3680,.F.);
#4954=ORIENTED_EDGE('',*,*,#3681,.F.);
#4955=ORIENTED_EDGE('',*,*,#3675,.T.);
#4956=ORIENTED_EDGE('',*,*,#3681,.T.);
#4957=ORIENTED_EDGE('',*,*,#3682,.T.);
#4958=ORIENTED_EDGE('',*,*,#3683,.T.);
#4959=ORIENTED_EDGE('',*,*,#3677,.T.);
#4960=ORIENTED_EDGE('',*,*,#3684,.T.);
#4961=ORIENTED_EDGE('',*,*,#3685,.T.);
#4962=ORIENTED_EDGE('',*,*,#3614,.F.);
#4963=ORIENTED_EDGE('',*,*,#3676,.T.);
#4964=ORIENTED_EDGE('',*,*,#3683,.F.);
#4965=ORIENTED_EDGE('',*,*,#3686,.F.);
#4966=ORIENTED_EDGE('',*,*,#3684,.F.);
#4967=ORIENTED_EDGE('',*,*,#3687,.T.);
#4968=ORIENTED_EDGE('',*,*,#3688,.T.);
#4969=ORIENTED_EDGE('',*,*,#3686,.T.);
#4970=ORIENTED_EDGE('',*,*,#3689,.T.);
#4971=ORIENTED_EDGE('',*,*,#3690,.T.);
#4972=ORIENTED_EDGE('',*,*,#3691,.T.);
#4973=ORIENTED_EDGE('',*,*,#3680,.T.);
#4974=ORIENTED_EDGE('',*,*,#3692,.T.);
#4975=ORIENTED_EDGE('',*,*,#3693,.T.);
#4976=ORIENTED_EDGE('',*,*,#3687,.F.);
#4977=ORIENTED_EDGE('',*,*,#3682,.F.);
#4978=ORIENTED_EDGE('',*,*,#3693,.F.);
#4979=ORIENTED_EDGE('',*,*,#3604,.F.);
#4980=ORIENTED_EDGE('',*,*,#3625,.F.);
#4981=ORIENTED_EDGE('',*,*,#3605,.F.);
#4982=ORIENTED_EDGE('',*,*,#3692,.F.);
#4983=ORIENTED_EDGE('',*,*,#3678,.F.);
#4984=ORIENTED_EDGE('',*,*,#3694,.T.);
#4985=ORIENTED_EDGE('',*,*,#3651,.T.);
#4986=ORIENTED_EDGE('',*,*,#3695,.T.);
#4987=ORIENTED_EDGE('',*,*,#3695,.F.);
#4988=ORIENTED_EDGE('',*,*,#3654,.F.);
#4989=ORIENTED_EDGE('',*,*,#3691,.F.);
#4990=ORIENTED_EDGE('',*,*,#3696,.F.);
#4991=ORIENTED_EDGE('',*,*,#3633,.F.);
#4992=ORIENTED_EDGE('',*,*,#3648,.F.);
#4993=ORIENTED_EDGE('',*,*,#3694,.F.);
#4994=ORIENTED_EDGE('',*,*,#3697,.F.);
#4995=ORIENTED_EDGE('',*,*,#3635,.F.);
#4996=ORIENTED_EDGE('',*,*,#3698,.F.);
#4997=ORIENTED_EDGE('',*,*,#3690,.F.);
#4998=ORIENTED_EDGE('',*,*,#3656,.F.);
#4999=ORIENTED_EDGE('',*,*,#3643,.T.);
#5000=ORIENTED_EDGE('',*,*,#3657,.F.);
#5001=ORIENTED_EDGE('',*,*,#3689,.F.);
#5002=ORIENTED_EDGE('',*,*,#3653,.F.);
#5003=ORIENTED_EDGE('',*,*,#3615,.F.);
#5004=ORIENTED_EDGE('',*,*,#3685,.F.);
#5005=ORIENTED_EDGE('',*,*,#3688,.F.);
#5006=ORIENTED_EDGE('',*,*,#3603,.F.);
#5007=ORIENTED_EDGE('',*,*,#3697,.T.);
#5008=ORIENTED_EDGE('',*,*,#3696,.T.);
#5009=ORIENTED_EDGE('',*,*,#3698,.T.);
#5010=ORIENTED_EDGE('',*,*,#3634,.F.);
#5011=ORIENTED_EDGE('',*,*,#3699,.F.);
#5012=ORIENTED_EDGE('',*,*,#3700,.F.);
#5013=ORIENTED_EDGE('',*,*,#3701,.F.);
#5014=ORIENTED_EDGE('',*,*,#3702,.F.);
#5015=ORIENTED_EDGE('',*,*,#3703,.F.);
#5016=ORIENTED_EDGE('',*,*,#3704,.F.);
#5017=ORIENTED_EDGE('',*,*,#3705,.F.);
#5018=ORIENTED_EDGE('',*,*,#3706,.F.);
#5019=ORIENTED_EDGE('',*,*,#3707,.F.);
#5020=ORIENTED_EDGE('',*,*,#3699,.T.);
#5021=ORIENTED_EDGE('',*,*,#3708,.T.);
#5022=ORIENTED_EDGE('',*,*,#3706,.T.);
#5023=ORIENTED_EDGE('',*,*,#3709,.T.);
#5024=ORIENTED_EDGE('',*,*,#3623,.T.);
#5025=ORIENTED_EDGE('',*,*,#3710,.T.);
#5026=ORIENTED_EDGE('',*,*,#3707,.T.);
#5027=ORIENTED_EDGE('',*,*,#3711,.T.);
#5028=ORIENTED_EDGE('',*,*,#3712,.F.);
#5029=ORIENTED_EDGE('',*,*,#3713,.F.);
#5030=ORIENTED_EDGE('',*,*,#3714,.F.);
#5031=ORIENTED_EDGE('',*,*,#3713,.T.);
#5032=ORIENTED_EDGE('',*,*,#3715,.T.);
#5033=ORIENTED_EDGE('',*,*,#3703,.T.);
#5034=ORIENTED_EDGE('',*,*,#3716,.T.);
#5035=ORIENTED_EDGE('',*,*,#3705,.T.);
#5036=ORIENTED_EDGE('',*,*,#3717,.T.);
#5037=ORIENTED_EDGE('',*,*,#3714,.T.);
#5038=ORIENTED_EDGE('',*,*,#3718,.T.);
#5039=ORIENTED_EDGE('',*,*,#3621,.T.);
#5040=ORIENTED_EDGE('',*,*,#3719,.T.);
#5041=ORIENTED_EDGE('',*,*,#3712,.T.);
#5042=ORIENTED_EDGE('',*,*,#3720,.T.);
#5043=ORIENTED_EDGE('',*,*,#3619,.T.);
#5044=ORIENTED_EDGE('',*,*,#3721,.T.);
#5045=ORIENTED_EDGE('',*,*,#3704,.T.);
#5046=ORIENTED_EDGE('',*,*,#3722,.T.);
#5047=ORIENTED_EDGE('',*,*,#3702,.T.);
#5048=ORIENTED_EDGE('',*,*,#3723,.T.);
#5049=ORIENTED_EDGE('',*,*,#3700,.T.);
#5050=ORIENTED_EDGE('',*,*,#3724,.T.);
#5051=ORIENTED_EDGE('',*,*,#3617,.T.);
#5052=ORIENTED_EDGE('',*,*,#3725,.T.);
#5053=ORIENTED_EDGE('',*,*,#3701,.T.);
#5054=ORIENTED_EDGE('',*,*,#3726,.T.);
#5055=ORIENTED_EDGE('',*,*,#3720,.F.);
#5056=ORIENTED_EDGE('',*,*,#3717,.F.);
#5057=ORIENTED_EDGE('',*,*,#3710,.F.);
#5058=ORIENTED_EDGE('',*,*,#3622,.F.);
#5059=ORIENTED_EDGE('',*,*,#3536,.T.);
#5060=ORIENTED_EDGE('',*,*,#3624,.F.);
#5061=ORIENTED_EDGE('',*,*,#3711,.F.);
#5062=ORIENTED_EDGE('',*,*,#3708,.F.);
#5063=ORIENTED_EDGE('',*,*,#3725,.F.);
#5064=ORIENTED_EDGE('',*,*,#3616,.F.);
#5065=ORIENTED_EDGE('',*,*,#3552,.T.);
#5066=ORIENTED_EDGE('',*,*,#3565,.T.);
#5067=ORIENTED_EDGE('',*,*,#3716,.F.);
#5068=ORIENTED_EDGE('',*,*,#3724,.F.);
#5069=ORIENTED_EDGE('',*,*,#3709,.F.);
#5070=ORIENTED_EDGE('',*,*,#3718,.F.);
#5071=ORIENTED_EDGE('',*,*,#3526,.T.);
#5072=ORIENTED_EDGE('',*,*,#3522,.T.);
#5073=ORIENTED_EDGE('',*,*,#3519,.T.);
#5074=ORIENTED_EDGE('',*,*,#3517,.T.);
#5075=ORIENTED_EDGE('',*,*,#3515,.T.);
#5076=ORIENTED_EDGE('',*,*,#3512,.T.);
#5077=ORIENTED_EDGE('',*,*,#3721,.F.);
#5078=ORIENTED_EDGE('',*,*,#3618,.F.);
#5079=ORIENTED_EDGE('',*,*,#3726,.F.);
#5080=ORIENTED_EDGE('',*,*,#3723,.F.);
#5081=ORIENTED_EDGE('',*,*,#3719,.F.);
#5082=ORIENTED_EDGE('',*,*,#3620,.F.);
#5083=ORIENTED_EDGE('',*,*,#3722,.F.);
#5084=ORIENTED_EDGE('',*,*,#3715,.F.);
#5085=ORIENTED_EDGE('',*,*,#3727,.T.);
#5086=ORIENTED_EDGE('',*,*,#3728,.T.);
#5087=ORIENTED_EDGE('',*,*,#3729,.T.);
#5088=ORIENTED_EDGE('',*,*,#3730,.F.);
#5089=ORIENTED_EDGE('',*,*,#3731,.T.);
#5090=ORIENTED_EDGE('',*,*,#3732,.T.);
#5091=ORIENTED_EDGE('',*,*,#3733,.T.);
#5092=ORIENTED_EDGE('',*,*,#3734,.F.);
#5093=ORIENTED_EDGE('',*,*,#3735,.T.);
#5094=ORIENTED_EDGE('',*,*,#3736,.T.);
#5095=ORIENTED_EDGE('',*,*,#3737,.T.);
#5096=ORIENTED_EDGE('',*,*,#3738,.F.);
#5097=ORIENTED_EDGE('',*,*,#3739,.T.);
#5098=ORIENTED_EDGE('',*,*,#3740,.F.);
#5099=ORIENTED_EDGE('',*,*,#3739,.F.);
#5100=ORIENTED_EDGE('',*,*,#3741,.F.);
#5101=ORIENTED_EDGE('',*,*,#3742,.T.);
#5102=ORIENTED_EDGE('',*,*,#3736,.F.);
#5103=ORIENTED_EDGE('',*,*,#3742,.F.);
#5104=ORIENTED_EDGE('',*,*,#3743,.F.);
#5105=ORIENTED_EDGE('',*,*,#3744,.T.);
#5106=ORIENTED_EDGE('',*,*,#3735,.F.);
#5107=ORIENTED_EDGE('',*,*,#3744,.F.);
#5108=ORIENTED_EDGE('',*,*,#3745,.F.);
#5109=ORIENTED_EDGE('',*,*,#3746,.T.);
#5110=ORIENTED_EDGE('',*,*,#3747,.F.);
#5111=ORIENTED_EDGE('',*,*,#3746,.F.);
#5112=ORIENTED_EDGE('',*,*,#3748,.F.);
#5113=ORIENTED_EDGE('',*,*,#3749,.T.);
#5114=ORIENTED_EDGE('',*,*,#3750,.T.);
#5115=ORIENTED_EDGE('',*,*,#3751,.F.);
#5116=ORIENTED_EDGE('',*,*,#3752,.F.);
#5117=ORIENTED_EDGE('',*,*,#3753,.T.);
#5118=ORIENTED_EDGE('',*,*,#3754,.T.);
#5119=ORIENTED_EDGE('',*,*,#3749,.F.);
#5120=ORIENTED_EDGE('',*,*,#3755,.F.);
#5121=ORIENTED_EDGE('',*,*,#3756,.T.);
#5122=ORIENTED_EDGE('',*,*,#3757,.T.);
#5123=ORIENTED_EDGE('',*,*,#3753,.F.);
#5124=ORIENTED_EDGE('',*,*,#3758,.F.);
#5125=ORIENTED_EDGE('',*,*,#3759,.T.);
#5126=ORIENTED_EDGE('',*,*,#3760,.T.);
#5127=ORIENTED_EDGE('',*,*,#3756,.F.);
#5128=ORIENTED_EDGE('',*,*,#3761,.F.);
#5129=ORIENTED_EDGE('',*,*,#3762,.T.);
#5130=ORIENTED_EDGE('',*,*,#3763,.T.);
#5131=ORIENTED_EDGE('',*,*,#3759,.F.);
#5132=ORIENTED_EDGE('',*,*,#3764,.F.);
#5133=ORIENTED_EDGE('',*,*,#3751,.T.);
#5134=ORIENTED_EDGE('',*,*,#3765,.T.);
#5135=ORIENTED_EDGE('',*,*,#3762,.F.);
#5136=ORIENTED_EDGE('',*,*,#3765,.F.);
#5137=ORIENTED_EDGE('',*,*,#3750,.F.);
#5138=ORIENTED_EDGE('',*,*,#3754,.F.);
#5139=ORIENTED_EDGE('',*,*,#3757,.F.);
#5140=ORIENTED_EDGE('',*,*,#3760,.F.);
#5141=ORIENTED_EDGE('',*,*,#3763,.F.);
#5142=ORIENTED_EDGE('',*,*,#3766,.F.);
#5143=ORIENTED_EDGE('',*,*,#3767,.F.);
#5144=ORIENTED_EDGE('',*,*,#3768,.T.);
#5145=ORIENTED_EDGE('',*,*,#3769,.T.);
#5146=ORIENTED_EDGE('',*,*,#3770,.F.);
#5147=ORIENTED_EDGE('',*,*,#3771,.F.);
#5148=ORIENTED_EDGE('',*,*,#3772,.T.);
#5149=ORIENTED_EDGE('',*,*,#3773,.T.);
#5150=ORIENTED_EDGE('',*,*,#3768,.F.);
#5151=ORIENTED_EDGE('',*,*,#3774,.F.);
#5152=ORIENTED_EDGE('',*,*,#3775,.T.);
#5153=ORIENTED_EDGE('',*,*,#3776,.T.);
#5154=ORIENTED_EDGE('',*,*,#3772,.F.);
#5155=ORIENTED_EDGE('',*,*,#3777,.F.);
#5156=ORIENTED_EDGE('',*,*,#3778,.T.);
#5157=ORIENTED_EDGE('',*,*,#3779,.T.);
#5158=ORIENTED_EDGE('',*,*,#3775,.F.);
#5159=ORIENTED_EDGE('',*,*,#3780,.F.);
#5160=ORIENTED_EDGE('',*,*,#3781,.T.);
#5161=ORIENTED_EDGE('',*,*,#3782,.T.);
#5162=ORIENTED_EDGE('',*,*,#3778,.F.);
#5163=ORIENTED_EDGE('',*,*,#3783,.F.);
#5164=ORIENTED_EDGE('',*,*,#3770,.T.);
#5165=ORIENTED_EDGE('',*,*,#3784,.T.);
#5166=ORIENTED_EDGE('',*,*,#3781,.F.);
#5167=ORIENTED_EDGE('',*,*,#3784,.F.);
#5168=ORIENTED_EDGE('',*,*,#3769,.F.);
#5169=ORIENTED_EDGE('',*,*,#3773,.F.);
#5170=ORIENTED_EDGE('',*,*,#3776,.F.);
#5171=ORIENTED_EDGE('',*,*,#3779,.F.);
#5172=ORIENTED_EDGE('',*,*,#3782,.F.);
#5173=ORIENTED_EDGE('',*,*,#3785,.F.);
#5174=ORIENTED_EDGE('',*,*,#3785,.T.);
#5175=ORIENTED_EDGE('',*,*,#3786,.T.);
#5176=ORIENTED_EDGE('',*,*,#3787,.F.);
#5177=ORIENTED_EDGE('',*,*,#3786,.F.);
#5178=ORIENTED_EDGE('',*,*,#3766,.T.);
#5179=ORIENTED_EDGE('',*,*,#3788,.T.);
#5180=ORIENTED_EDGE('',*,*,#3789,.F.);
#5181=ORIENTED_EDGE('',*,*,#3788,.F.);
#5182=ORIENTED_EDGE('',*,*,#3790,.F.);
#5183=ORIENTED_EDGE('',*,*,#3791,.F.);
#5184=ORIENTED_EDGE('',*,*,#3792,.F.);
#5185=ORIENTED_EDGE('',*,*,#3793,.T.);
#5186=ORIENTED_EDGE('',*,*,#3794,.F.);
#5187=ORIENTED_EDGE('',*,*,#3795,.T.);
#5188=ORIENTED_EDGE('',*,*,#3796,.F.);
#5189=ORIENTED_EDGE('',*,*,#3797,.F.);
#5190=ORIENTED_EDGE('',*,*,#3798,.F.);
#5191=ORIENTED_EDGE('',*,*,#3799,.T.);
#5192=ORIENTED_EDGE('',*,*,#3800,.F.);
#5193=ORIENTED_EDGE('',*,*,#3801,.F.);
#5194=ORIENTED_EDGE('',*,*,#3802,.F.);
#5195=ORIENTED_EDGE('',*,*,#3803,.T.);
#5196=ORIENTED_EDGE('',*,*,#3804,.F.);
#5197=ORIENTED_EDGE('',*,*,#3805,.F.);
#5198=ORIENTED_EDGE('',*,*,#3806,.F.);
#5199=ORIENTED_EDGE('',*,*,#3807,.T.);
#5200=ORIENTED_EDGE('',*,*,#3808,.F.);
#5201=ORIENTED_EDGE('',*,*,#3809,.F.);
#5202=ORIENTED_EDGE('',*,*,#3810,.F.);
#5203=ORIENTED_EDGE('',*,*,#3811,.F.);
#5204=ORIENTED_EDGE('',*,*,#3812,.F.);
#5205=ORIENTED_EDGE('',*,*,#3813,.T.);
#5206=ORIENTED_EDGE('',*,*,#3814,.F.);
#5207=ORIENTED_EDGE('',*,*,#3815,.F.);
#5208=ORIENTED_EDGE('',*,*,#3816,.F.);
#5209=ORIENTED_EDGE('',*,*,#3817,.T.);
#5210=ORIENTED_EDGE('',*,*,#3818,.F.);
#5211=ORIENTED_EDGE('',*,*,#3787,.T.);
#5212=ORIENTED_EDGE('',*,*,#3819,.F.);
#5213=ORIENTED_EDGE('',*,*,#3789,.T.);
#5214=ORIENTED_EDGE('',*,*,#3820,.F.);
#5215=ORIENTED_EDGE('',*,*,#3793,.F.);
#5216=ORIENTED_EDGE('',*,*,#3821,.F.);
#5217=ORIENTED_EDGE('',*,*,#3807,.F.);
#5218=ORIENTED_EDGE('',*,*,#3822,.F.);
#5219=ORIENTED_EDGE('',*,*,#3813,.F.);
#5220=ORIENTED_EDGE('',*,*,#3823,.F.);
#5221=ORIENTED_EDGE('',*,*,#3795,.F.);
#5222=ORIENTED_EDGE('',*,*,#3824,.F.);
#5223=ORIENTED_EDGE('',*,*,#3817,.F.);
#5224=ORIENTED_EDGE('',*,*,#3825,.F.);
#5225=ORIENTED_EDGE('',*,*,#3799,.F.);
#5226=ORIENTED_EDGE('',*,*,#3826,.F.);
#5227=ORIENTED_EDGE('',*,*,#3827,.F.);
#5228=ORIENTED_EDGE('',*,*,#3828,.F.);
#5229=ORIENTED_EDGE('',*,*,#3803,.F.);
#5230=ORIENTED_EDGE('',*,*,#3829,.F.);
#5231=ORIENTED_EDGE('',*,*,#3830,.F.);
#5232=ORIENTED_EDGE('',*,*,#3831,.F.);
#5233=ORIENTED_EDGE('',*,*,#3827,.T.);
#5234=ORIENTED_EDGE('',*,*,#3832,.T.);
#5235=ORIENTED_EDGE('',*,*,#3833,.F.);
#5236=ORIENTED_EDGE('',*,*,#3834,.F.);
#5237=ORIENTED_EDGE('',*,*,#3835,.F.);
#5238=ORIENTED_EDGE('',*,*,#3836,.F.);
#5239=ORIENTED_EDGE('',*,*,#3837,.F.);
#5240=ORIENTED_EDGE('',*,*,#3804,.T.);
#5241=ORIENTED_EDGE('',*,*,#3828,.T.);
#5242=ORIENTED_EDGE('',*,*,#3831,.T.);
#5243=ORIENTED_EDGE('',*,*,#3838,.T.);
#5244=ORIENTED_EDGE('',*,*,#3839,.F.);
#5245=ORIENTED_EDGE('',*,*,#3840,.F.);
#5246=ORIENTED_EDGE('',*,*,#3841,.F.);
#5247=ORIENTED_EDGE('',*,*,#3842,.F.);
#5248=ORIENTED_EDGE('',*,*,#3843,.F.);
#5249=ORIENTED_EDGE('',*,*,#3844,.T.);
#5250=ORIENTED_EDGE('',*,*,#3800,.T.);
#5251=ORIENTED_EDGE('',*,*,#3825,.T.);
#5252=ORIENTED_EDGE('',*,*,#3816,.T.);
#5253=ORIENTED_EDGE('',*,*,#3845,.T.);
#5254=ORIENTED_EDGE('',*,*,#3846,.F.);
#5255=ORIENTED_EDGE('',*,*,#3847,.F.);
#5256=ORIENTED_EDGE('',*,*,#3848,.F.);
#5257=ORIENTED_EDGE('',*,*,#3849,.F.);
#5258=ORIENTED_EDGE('',*,*,#3850,.F.);
#5259=ORIENTED_EDGE('',*,*,#3851,.T.);
#5260=ORIENTED_EDGE('',*,*,#3796,.T.);
#5261=ORIENTED_EDGE('',*,*,#3823,.T.);
#5262=ORIENTED_EDGE('',*,*,#3812,.T.);
#5263=ORIENTED_EDGE('',*,*,#3852,.T.);
#5264=ORIENTED_EDGE('',*,*,#3853,.F.);
#5265=ORIENTED_EDGE('',*,*,#3854,.F.);
#5266=ORIENTED_EDGE('',*,*,#3732,.F.);
#5267=ORIENTED_EDGE('',*,*,#3855,.F.);
#5268=ORIENTED_EDGE('',*,*,#3856,.F.);
#5269=ORIENTED_EDGE('',*,*,#3857,.T.);
#5270=ORIENTED_EDGE('',*,*,#3790,.T.);
#5271=ORIENTED_EDGE('',*,*,#3820,.T.);
#5272=ORIENTED_EDGE('',*,*,#3806,.T.);
#5273=ORIENTED_EDGE('',*,*,#3858,.F.);
#5274=ORIENTED_EDGE('',*,*,#3859,.T.);
#5275=ORIENTED_EDGE('',*,*,#3860,.T.);
#5276=ORIENTED_EDGE('',*,*,#3861,.T.);
#5277=ORIENTED_EDGE('',*,*,#3862,.F.);
#5278=ORIENTED_EDGE('',*,*,#3805,.T.);
#5279=ORIENTED_EDGE('',*,*,#3844,.F.);
#5280=ORIENTED_EDGE('',*,*,#3863,.T.);
#5281=ORIENTED_EDGE('',*,*,#3832,.F.);
#5282=ORIENTED_EDGE('',*,*,#3864,.T.);
#5283=ORIENTED_EDGE('',*,*,#3838,.F.);
#5284=ORIENTED_EDGE('',*,*,#3830,.T.);
#5285=ORIENTED_EDGE('',*,*,#3865,.F.);
#5286=ORIENTED_EDGE('',*,*,#3866,.T.);
#5287=ORIENTED_EDGE('',*,*,#3845,.F.);
#5288=ORIENTED_EDGE('',*,*,#3815,.T.);
#5289=ORIENTED_EDGE('',*,*,#3867,.F.);
#5290=ORIENTED_EDGE('',*,*,#3868,.T.);
#5291=ORIENTED_EDGE('',*,*,#3852,.F.);
#5292=ORIENTED_EDGE('',*,*,#3811,.T.);
#5293=ORIENTED_EDGE('',*,*,#3869,.F.);
#5294=ORIENTED_EDGE('',*,*,#3870,.T.);
#5295=ORIENTED_EDGE('',*,*,#3871,.T.);
#5296=ORIENTED_EDGE('',*,*,#3858,.T.);
#5297=ORIENTED_EDGE('',*,*,#3809,.T.);
#5298=ORIENTED_EDGE('',*,*,#3872,.T.);
#5299=ORIENTED_EDGE('',*,*,#3873,.F.);
#5300=ORIENTED_EDGE('',*,*,#3874,.T.);
#5301=ORIENTED_EDGE('',*,*,#3875,.F.);
#5302=ORIENTED_EDGE('',*,*,#3876,.T.);
#5303=ORIENTED_EDGE('',*,*,#3877,.F.);
#5304=ORIENTED_EDGE('',*,*,#3878,.T.);
#5305=ORIENTED_EDGE('',*,*,#3879,.F.);
#5306=ORIENTED_EDGE('',*,*,#3880,.T.);
#5307=ORIENTED_EDGE('',*,*,#3791,.T.);
#5308=ORIENTED_EDGE('',*,*,#3862,.T.);
#5309=ORIENTED_EDGE('',*,*,#3881,.T.);
#5310=ORIENTED_EDGE('',*,*,#3882,.T.);
#5311=ORIENTED_EDGE('',*,*,#3883,.F.);
#5312=ORIENTED_EDGE('',*,*,#3797,.T.);
#5313=ORIENTED_EDGE('',*,*,#3857,.F.);
#5314=ORIENTED_EDGE('',*,*,#3884,.T.);
#5315=ORIENTED_EDGE('',*,*,#3885,.F.);
#5316=ORIENTED_EDGE('',*,*,#3801,.T.);
#5317=ORIENTED_EDGE('',*,*,#3851,.F.);
#5318=ORIENTED_EDGE('',*,*,#3886,.T.);
#5319=ORIENTED_EDGE('',*,*,#3887,.F.);
#5320=ORIENTED_EDGE('',*,*,#3888,.T.);
#5321=ORIENTED_EDGE('',*,*,#3889,.T.);
#5322=ORIENTED_EDGE('',*,*,#3890,.T.);
#5323=ORIENTED_EDGE('',*,*,#3891,.T.);
#5324=ORIENTED_EDGE('',*,*,#3892,.T.);
#5325=ORIENTED_EDGE('',*,*,#3893,.F.);
#5326=ORIENTED_EDGE('',*,*,#3894,.F.);
#5327=ORIENTED_EDGE('',*,*,#3895,.T.);
#5328=ORIENTED_EDGE('',*,*,#3819,.T.);
#5329=ORIENTED_EDGE('',*,*,#3895,.F.);
#5330=ORIENTED_EDGE('',*,*,#3737,.F.);
#5331=ORIENTED_EDGE('',*,*,#3896,.T.);
#5332=ORIENTED_EDGE('',*,*,#3818,.T.);
#5333=ORIENTED_EDGE('',*,*,#3896,.F.);
#5334=ORIENTED_EDGE('',*,*,#3897,.F.);
#5335=ORIENTED_EDGE('',*,*,#3893,.T.);
#5336=ORIENTED_EDGE('',*,*,#3898,.F.);
#5337=ORIENTED_EDGE('',*,*,#3899,.F.);
#5338=ORIENTED_EDGE('',*,*,#3900,.F.);
#5339=ORIENTED_EDGE('',*,*,#3901,.F.);
#5340=ORIENTED_EDGE('',*,*,#3833,.T.);
#5341=ORIENTED_EDGE('',*,*,#3863,.F.);
#5342=ORIENTED_EDGE('',*,*,#3843,.T.);
#5343=ORIENTED_EDGE('',*,*,#3902,.T.);
#5344=ORIENTED_EDGE('',*,*,#3897,.T.);
#5345=ORIENTED_EDGE('',*,*,#3903,.T.);
#5346=ORIENTED_EDGE('',*,*,#3904,.T.);
#5347=ORIENTED_EDGE('',*,*,#3888,.F.);
#5348=ORIENTED_EDGE('',*,*,#3834,.T.);
#5349=ORIENTED_EDGE('',*,*,#3902,.F.);
#5350=ORIENTED_EDGE('',*,*,#3842,.T.);
#5351=ORIENTED_EDGE('',*,*,#3905,.F.);
#5352=ORIENTED_EDGE('',*,*,#3901,.T.);
#5353=ORIENTED_EDGE('',*,*,#3906,.F.);
#5354=ORIENTED_EDGE('',*,*,#3907,.F.);
#5355=ORIENTED_EDGE('',*,*,#3903,.F.);
#5356=ORIENTED_EDGE('',*,*,#3835,.T.);
#5357=ORIENTED_EDGE('',*,*,#3905,.T.);
#5358=ORIENTED_EDGE('',*,*,#3841,.T.);
#5359=ORIENTED_EDGE('',*,*,#3908,.T.);
#5360=ORIENTED_EDGE('',*,*,#3740,.T.);
#5361=ORIENTED_EDGE('',*,*,#3747,.T.);
#5362=ORIENTED_EDGE('',*,*,#3894,.T.);
#5363=ORIENTED_EDGE('',*,*,#3900,.T.);
#5364=ORIENTED_EDGE('',*,*,#3909,.T.);
#5365=ORIENTED_EDGE('',*,*,#3910,.T.);
#5366=ORIENTED_EDGE('',*,*,#3906,.T.);
#5367=ORIENTED_EDGE('',*,*,#3836,.T.);
#5368=ORIENTED_EDGE('',*,*,#3908,.F.);
#5369=ORIENTED_EDGE('',*,*,#3840,.T.);
#5370=ORIENTED_EDGE('',*,*,#3911,.F.);
#5371=ORIENTED_EDGE('',*,*,#3837,.T.);
#5372=ORIENTED_EDGE('',*,*,#3911,.T.);
#5373=ORIENTED_EDGE('',*,*,#3839,.T.);
#5374=ORIENTED_EDGE('',*,*,#3864,.F.);
#5375=ORIENTED_EDGE('',*,*,#3898,.T.);
#5376=ORIENTED_EDGE('',*,*,#3892,.F.);
#5377=ORIENTED_EDGE('',*,*,#3912,.T.);
#5378=ORIENTED_EDGE('',*,*,#3913,.T.);
#5379=ORIENTED_EDGE('',*,*,#3802,.T.);
#5380=ORIENTED_EDGE('',*,*,#3887,.T.);
#5381=ORIENTED_EDGE('',*,*,#3914,.F.);
#5382=ORIENTED_EDGE('',*,*,#3915,.F.);
#5383=ORIENTED_EDGE('',*,*,#3916,.F.);
#5384=ORIENTED_EDGE('',*,*,#3917,.F.);
#5385=ORIENTED_EDGE('',*,*,#3918,.F.);
#5386=ORIENTED_EDGE('',*,*,#3865,.T.);
#5387=ORIENTED_EDGE('',*,*,#3829,.T.);
#5388=ORIENTED_EDGE('',*,*,#3826,.T.);
#5389=ORIENTED_EDGE('',*,*,#3914,.T.);
#5390=ORIENTED_EDGE('',*,*,#3886,.F.);
#5391=ORIENTED_EDGE('',*,*,#3850,.T.);
#5392=ORIENTED_EDGE('',*,*,#3919,.T.);
#5393=ORIENTED_EDGE('',*,*,#3915,.T.);
#5394=ORIENTED_EDGE('',*,*,#3919,.F.);
#5395=ORIENTED_EDGE('',*,*,#3849,.T.);
#5396=ORIENTED_EDGE('',*,*,#3920,.F.);
#5397=ORIENTED_EDGE('',*,*,#3916,.T.);
#5398=ORIENTED_EDGE('',*,*,#3920,.T.);
#5399=ORIENTED_EDGE('',*,*,#3848,.T.);
#5400=ORIENTED_EDGE('',*,*,#3921,.T.);
#5401=ORIENTED_EDGE('',*,*,#3917,.T.);
#5402=ORIENTED_EDGE('',*,*,#3921,.F.);
#5403=ORIENTED_EDGE('',*,*,#3847,.T.);
#5404=ORIENTED_EDGE('',*,*,#3922,.F.);
#5405=ORIENTED_EDGE('',*,*,#3918,.T.);
#5406=ORIENTED_EDGE('',*,*,#3922,.T.);
#5407=ORIENTED_EDGE('',*,*,#3846,.T.);
#5408=ORIENTED_EDGE('',*,*,#3866,.F.);
#5409=ORIENTED_EDGE('',*,*,#3798,.T.);
#5410=ORIENTED_EDGE('',*,*,#3885,.T.);
#5411=ORIENTED_EDGE('',*,*,#3923,.F.);
#5412=ORIENTED_EDGE('',*,*,#3924,.F.);
#5413=ORIENTED_EDGE('',*,*,#3728,.F.);
#5414=ORIENTED_EDGE('',*,*,#3925,.F.);
#5415=ORIENTED_EDGE('',*,*,#3926,.F.);
#5416=ORIENTED_EDGE('',*,*,#3867,.T.);
#5417=ORIENTED_EDGE('',*,*,#3814,.T.);
#5418=ORIENTED_EDGE('',*,*,#3824,.T.);
#5419=ORIENTED_EDGE('',*,*,#3923,.T.);
#5420=ORIENTED_EDGE('',*,*,#3884,.F.);
#5421=ORIENTED_EDGE('',*,*,#3856,.T.);
#5422=ORIENTED_EDGE('',*,*,#3927,.T.);
#5423=ORIENTED_EDGE('',*,*,#3730,.T.);
#5424=ORIENTED_EDGE('',*,*,#3729,.F.);
#5425=ORIENTED_EDGE('',*,*,#3924,.T.);
#5426=ORIENTED_EDGE('',*,*,#3927,.F.);
#5427=ORIENTED_EDGE('',*,*,#3855,.T.);
#5428=ORIENTED_EDGE('',*,*,#3731,.F.);
#5429=ORIENTED_EDGE('',*,*,#3734,.T.);
#5430=ORIENTED_EDGE('',*,*,#3733,.F.);
#5431=ORIENTED_EDGE('',*,*,#3854,.T.);
#5432=ORIENTED_EDGE('',*,*,#3928,.F.);
#5433=ORIENTED_EDGE('',*,*,#3925,.T.);
#5434=ORIENTED_EDGE('',*,*,#3727,.F.);
#5435=ORIENTED_EDGE('',*,*,#3926,.T.);
#5436=ORIENTED_EDGE('',*,*,#3928,.T.);
#5437=ORIENTED_EDGE('',*,*,#3853,.T.);
#5438=ORIENTED_EDGE('',*,*,#3868,.F.);
#5439=ORIENTED_EDGE('',*,*,#3794,.T.);
#5440=ORIENTED_EDGE('',*,*,#3883,.T.);
#5441=ORIENTED_EDGE('',*,*,#3929,.F.);
#5442=ORIENTED_EDGE('',*,*,#3930,.F.);
#5443=ORIENTED_EDGE('',*,*,#3931,.F.);
#5444=ORIENTED_EDGE('',*,*,#3932,.F.);
#5445=ORIENTED_EDGE('',*,*,#3933,.F.);
#5446=ORIENTED_EDGE('',*,*,#3869,.T.);
#5447=ORIENTED_EDGE('',*,*,#3810,.T.);
#5448=ORIENTED_EDGE('',*,*,#3822,.T.);
#5449=ORIENTED_EDGE('',*,*,#3929,.T.);
#5450=ORIENTED_EDGE('',*,*,#3882,.F.);
#5451=ORIENTED_EDGE('',*,*,#3934,.T.);
#5452=ORIENTED_EDGE('',*,*,#3935,.T.);
#5453=ORIENTED_EDGE('',*,*,#3930,.T.);
#5454=ORIENTED_EDGE('',*,*,#3935,.F.);
#5455=ORIENTED_EDGE('',*,*,#3936,.F.);
#5456=ORIENTED_EDGE('',*,*,#3937,.F.);
#5457=ORIENTED_EDGE('',*,*,#3931,.T.);
#5458=ORIENTED_EDGE('',*,*,#3937,.T.);
#5459=ORIENTED_EDGE('',*,*,#3938,.T.);
#5460=ORIENTED_EDGE('',*,*,#3939,.T.);
#5461=ORIENTED_EDGE('',*,*,#3933,.T.);
#5462=ORIENTED_EDGE('',*,*,#3940,.T.);
#5463=ORIENTED_EDGE('',*,*,#3941,.T.);
#5464=ORIENTED_EDGE('',*,*,#3870,.F.);
#5465=ORIENTED_EDGE('',*,*,#3932,.T.);
#5466=ORIENTED_EDGE('',*,*,#3939,.F.);
#5467=ORIENTED_EDGE('',*,*,#3942,.F.);
#5468=ORIENTED_EDGE('',*,*,#3940,.F.);
#5469=ORIENTED_EDGE('',*,*,#3943,.T.);
#5470=ORIENTED_EDGE('',*,*,#3944,.T.);
#5471=ORIENTED_EDGE('',*,*,#3942,.T.);
#5472=ORIENTED_EDGE('',*,*,#3945,.T.);
#5473=ORIENTED_EDGE('',*,*,#3946,.T.);
#5474=ORIENTED_EDGE('',*,*,#3947,.T.);
#5475=ORIENTED_EDGE('',*,*,#3936,.T.);
#5476=ORIENTED_EDGE('',*,*,#3948,.T.);
#5477=ORIENTED_EDGE('',*,*,#3949,.T.);
#5478=ORIENTED_EDGE('',*,*,#3943,.F.);
#5479=ORIENTED_EDGE('',*,*,#3938,.F.);
#5480=ORIENTED_EDGE('',*,*,#3949,.F.);
#5481=ORIENTED_EDGE('',*,*,#3860,.F.);
#5482=ORIENTED_EDGE('',*,*,#3881,.F.);
#5483=ORIENTED_EDGE('',*,*,#3861,.F.);
#5484=ORIENTED_EDGE('',*,*,#3948,.F.);
#5485=ORIENTED_EDGE('',*,*,#3934,.F.);
#5486=ORIENTED_EDGE('',*,*,#3950,.T.);
#5487=ORIENTED_EDGE('',*,*,#3907,.T.);
#5488=ORIENTED_EDGE('',*,*,#3951,.T.);
#5489=ORIENTED_EDGE('',*,*,#3951,.F.);
#5490=ORIENTED_EDGE('',*,*,#3910,.F.);
#5491=ORIENTED_EDGE('',*,*,#3947,.F.);
#5492=ORIENTED_EDGE('',*,*,#3952,.F.);
#5493=ORIENTED_EDGE('',*,*,#3889,.F.);
#5494=ORIENTED_EDGE('',*,*,#3904,.F.);
#5495=ORIENTED_EDGE('',*,*,#3950,.F.);
#5496=ORIENTED_EDGE('',*,*,#3953,.F.);
#5497=ORIENTED_EDGE('',*,*,#3891,.F.);
#5498=ORIENTED_EDGE('',*,*,#3954,.F.);
#5499=ORIENTED_EDGE('',*,*,#3946,.F.);
#5500=ORIENTED_EDGE('',*,*,#3912,.F.);
#5501=ORIENTED_EDGE('',*,*,#3899,.T.);
#5502=ORIENTED_EDGE('',*,*,#3913,.F.);
#5503=ORIENTED_EDGE('',*,*,#3945,.F.);
#5504=ORIENTED_EDGE('',*,*,#3909,.F.);
#5505=ORIENTED_EDGE('',*,*,#3871,.F.);
#5506=ORIENTED_EDGE('',*,*,#3941,.F.);
#5507=ORIENTED_EDGE('',*,*,#3944,.F.);
#5508=ORIENTED_EDGE('',*,*,#3859,.F.);
#5509=ORIENTED_EDGE('',*,*,#3953,.T.);
#5510=ORIENTED_EDGE('',*,*,#3952,.T.);
#5511=ORIENTED_EDGE('',*,*,#3954,.T.);
#5512=ORIENTED_EDGE('',*,*,#3890,.F.);
#5513=ORIENTED_EDGE('',*,*,#3955,.F.);
#5514=ORIENTED_EDGE('',*,*,#3956,.F.);
#5515=ORIENTED_EDGE('',*,*,#3957,.F.);
#5516=ORIENTED_EDGE('',*,*,#3958,.F.);
#5517=ORIENTED_EDGE('',*,*,#3959,.F.);
#5518=ORIENTED_EDGE('',*,*,#3960,.F.);
#5519=ORIENTED_EDGE('',*,*,#3961,.F.);
#5520=ORIENTED_EDGE('',*,*,#3962,.F.);
#5521=ORIENTED_EDGE('',*,*,#3963,.F.);
#5522=ORIENTED_EDGE('',*,*,#3955,.T.);
#5523=ORIENTED_EDGE('',*,*,#3964,.T.);
#5524=ORIENTED_EDGE('',*,*,#3962,.T.);
#5525=ORIENTED_EDGE('',*,*,#3965,.T.);
#5526=ORIENTED_EDGE('',*,*,#3879,.T.);
#5527=ORIENTED_EDGE('',*,*,#3966,.T.);
#5528=ORIENTED_EDGE('',*,*,#3963,.T.);
#5529=ORIENTED_EDGE('',*,*,#3967,.T.);
#5530=ORIENTED_EDGE('',*,*,#3968,.F.);
#5531=ORIENTED_EDGE('',*,*,#3969,.F.);
#5532=ORIENTED_EDGE('',*,*,#3970,.F.);
#5533=ORIENTED_EDGE('',*,*,#3969,.T.);
#5534=ORIENTED_EDGE('',*,*,#3971,.T.);
#5535=ORIENTED_EDGE('',*,*,#3959,.T.);
#5536=ORIENTED_EDGE('',*,*,#3972,.T.);
#5537=ORIENTED_EDGE('',*,*,#3961,.T.);
#5538=ORIENTED_EDGE('',*,*,#3973,.T.);
#5539=ORIENTED_EDGE('',*,*,#3970,.T.);
#5540=ORIENTED_EDGE('',*,*,#3974,.T.);
#5541=ORIENTED_EDGE('',*,*,#3877,.T.);
#5542=ORIENTED_EDGE('',*,*,#3975,.T.);
#5543=ORIENTED_EDGE('',*,*,#3968,.T.);
#5544=ORIENTED_EDGE('',*,*,#3976,.T.);
#5545=ORIENTED_EDGE('',*,*,#3875,.T.);
#5546=ORIENTED_EDGE('',*,*,#3977,.T.);
#5547=ORIENTED_EDGE('',*,*,#3960,.T.);
#5548=ORIENTED_EDGE('',*,*,#3978,.T.);
#5549=ORIENTED_EDGE('',*,*,#3958,.T.);
#5550=ORIENTED_EDGE('',*,*,#3979,.T.);
#5551=ORIENTED_EDGE('',*,*,#3956,.T.);
#5552=ORIENTED_EDGE('',*,*,#3980,.T.);
#5553=ORIENTED_EDGE('',*,*,#3873,.T.);
#5554=ORIENTED_EDGE('',*,*,#3981,.T.);
#5555=ORIENTED_EDGE('',*,*,#3957,.T.);
#5556=ORIENTED_EDGE('',*,*,#3982,.T.);
#5557=ORIENTED_EDGE('',*,*,#3976,.F.);
#5558=ORIENTED_EDGE('',*,*,#3973,.F.);
#5559=ORIENTED_EDGE('',*,*,#3966,.F.);
#5560=ORIENTED_EDGE('',*,*,#3878,.F.);
#5561=ORIENTED_EDGE('',*,*,#3792,.T.);
#5562=ORIENTED_EDGE('',*,*,#3880,.F.);
#5563=ORIENTED_EDGE('',*,*,#3967,.F.);
#5564=ORIENTED_EDGE('',*,*,#3964,.F.);
#5565=ORIENTED_EDGE('',*,*,#3981,.F.);
#5566=ORIENTED_EDGE('',*,*,#3872,.F.);
#5567=ORIENTED_EDGE('',*,*,#3808,.T.);
#5568=ORIENTED_EDGE('',*,*,#3821,.T.);
#5569=ORIENTED_EDGE('',*,*,#3972,.F.);
#5570=ORIENTED_EDGE('',*,*,#3980,.F.);
#5571=ORIENTED_EDGE('',*,*,#3965,.F.);
#5572=ORIENTED_EDGE('',*,*,#3974,.F.);
#5573=ORIENTED_EDGE('',*,*,#3767,.T.);
#5574=ORIENTED_EDGE('',*,*,#3783,.T.);
#5575=ORIENTED_EDGE('',*,*,#3780,.T.);
#5576=ORIENTED_EDGE('',*,*,#3777,.T.);
#5577=ORIENTED_EDGE('',*,*,#3774,.T.);
#5578=ORIENTED_EDGE('',*,*,#3771,.T.);
#5579=ORIENTED_EDGE('',*,*,#3748,.T.);
#5580=ORIENTED_EDGE('',*,*,#3764,.T.);
#5581=ORIENTED_EDGE('',*,*,#3761,.T.);
#5582=ORIENTED_EDGE('',*,*,#3758,.T.);
#5583=ORIENTED_EDGE('',*,*,#3755,.T.);
#5584=ORIENTED_EDGE('',*,*,#3752,.T.);
#5585=ORIENTED_EDGE('',*,*,#3745,.T.);
#5586=ORIENTED_EDGE('',*,*,#3743,.T.);
#5587=ORIENTED_EDGE('',*,*,#3741,.T.);
#5588=ORIENTED_EDGE('',*,*,#3738,.T.);
#5589=ORIENTED_EDGE('',*,*,#3977,.F.);
#5590=ORIENTED_EDGE('',*,*,#3874,.F.);
#5591=ORIENTED_EDGE('',*,*,#3982,.F.);
#5592=ORIENTED_EDGE('',*,*,#3979,.F.);
#5593=ORIENTED_EDGE('',*,*,#3975,.F.);
#5594=ORIENTED_EDGE('',*,*,#3876,.F.);
#5595=ORIENTED_EDGE('',*,*,#3978,.F.);
#5596=ORIENTED_EDGE('',*,*,#3971,.F.);
#5597=ORIENTED_EDGE('',*,*,#3983,.F.);
#5598=ORIENTED_EDGE('',*,*,#3984,.T.);
#5599=ORIENTED_EDGE('',*,*,#3985,.F.);
#5600=ORIENTED_EDGE('',*,*,#3984,.F.);
#5601=ORIENTED_EDGE('',*,*,#3986,.F.);
#5602=ORIENTED_EDGE('',*,*,#3987,.T.);
#5603=ORIENTED_EDGE('',*,*,#3988,.F.);
#5604=ORIENTED_EDGE('',*,*,#3987,.F.);
#5605=ORIENTED_EDGE('',*,*,#3989,.T.);
#5606=ORIENTED_EDGE('',*,*,#3990,.T.);
#5607=ORIENTED_EDGE('',*,*,#3991,.F.);
#5608=ORIENTED_EDGE('',*,*,#3992,.T.);
#5609=ORIENTED_EDGE('',*,*,#3989,.F.);
#5610=ORIENTED_EDGE('',*,*,#3992,.F.);
#5611=ORIENTED_EDGE('',*,*,#3991,.T.);
#5612=ORIENTED_EDGE('',*,*,#3993,.T.);
#5613=ORIENTED_EDGE('',*,*,#3994,.T.);
#5614=ORIENTED_EDGE('',*,*,#3995,.F.);
#5615=ORIENTED_EDGE('',*,*,#3996,.T.);
#5616=ORIENTED_EDGE('',*,*,#3993,.F.);
#5617=ORIENTED_EDGE('',*,*,#3996,.F.);
#5618=ORIENTED_EDGE('',*,*,#3995,.T.);
#5619=ORIENTED_EDGE('',*,*,#3997,.T.);
#5620=ORIENTED_EDGE('',*,*,#3998,.T.);
#5621=ORIENTED_EDGE('',*,*,#3999,.F.);
#5622=ORIENTED_EDGE('',*,*,#4000,.T.);
#5623=ORIENTED_EDGE('',*,*,#3997,.F.);
#5624=ORIENTED_EDGE('',*,*,#4000,.F.);
#5625=ORIENTED_EDGE('',*,*,#3999,.T.);
#5626=ORIENTED_EDGE('',*,*,#4001,.T.);
#5627=ORIENTED_EDGE('',*,*,#4002,.T.);
#5628=ORIENTED_EDGE('',*,*,#4003,.F.);
#5629=ORIENTED_EDGE('',*,*,#4004,.T.);
#5630=ORIENTED_EDGE('',*,*,#4001,.F.);
#5631=ORIENTED_EDGE('',*,*,#4004,.F.);
#5632=ORIENTED_EDGE('',*,*,#4003,.T.);
#5633=ORIENTED_EDGE('',*,*,#3990,.F.);
#5634=ORIENTED_EDGE('',*,*,#4005,.T.);
#5635=ORIENTED_EDGE('',*,*,#4006,.F.);
#5636=ORIENTED_EDGE('',*,*,#4005,.F.);
#5637=ORIENTED_EDGE('',*,*,#3994,.F.);
#5638=ORIENTED_EDGE('',*,*,#4007,.T.);
#5639=ORIENTED_EDGE('',*,*,#4008,.F.);
#5640=ORIENTED_EDGE('',*,*,#4007,.F.);
#5641=ORIENTED_EDGE('',*,*,#3998,.F.);
#5642=ORIENTED_EDGE('',*,*,#4009,.T.);
#5643=ORIENTED_EDGE('',*,*,#4010,.F.);
#5644=ORIENTED_EDGE('',*,*,#4009,.F.);
#5645=ORIENTED_EDGE('',*,*,#4002,.F.);
#5646=ORIENTED_EDGE('',*,*,#4011,.T.);
#5647=ORIENTED_EDGE('',*,*,#4012,.F.);
#5648=ORIENTED_EDGE('',*,*,#4011,.F.);
#5649=ORIENTED_EDGE('',*,*,#4013,.T.);
#5650=ORIENTED_EDGE('',*,*,#4014,.T.);
#5651=ORIENTED_EDGE('',*,*,#4015,.T.);
#5652=ORIENTED_EDGE('',*,*,#4016,.T.);
#5653=ORIENTED_EDGE('',*,*,#4017,.T.);
#5654=ORIENTED_EDGE('',*,*,#4018,.T.);
#5655=ORIENTED_EDGE('',*,*,#4013,.F.);
#5656=ORIENTED_EDGE('',*,*,#4019,.T.);
#5657=ORIENTED_EDGE('',*,*,#4020,.T.);
#5658=ORIENTED_EDGE('',*,*,#4021,.T.);
#5659=ORIENTED_EDGE('',*,*,#4017,.F.);
#5660=ORIENTED_EDGE('',*,*,#4022,.T.);
#5661=ORIENTED_EDGE('',*,*,#4023,.T.);
#5662=ORIENTED_EDGE('',*,*,#4024,.T.);
#5663=ORIENTED_EDGE('',*,*,#4020,.F.);
#5664=ORIENTED_EDGE('',*,*,#4025,.T.);
#5665=ORIENTED_EDGE('',*,*,#4026,.T.);
#5666=ORIENTED_EDGE('',*,*,#4027,.T.);
#5667=ORIENTED_EDGE('',*,*,#4023,.F.);
#5668=ORIENTED_EDGE('',*,*,#4028,.T.);
#5669=ORIENTED_EDGE('',*,*,#4029,.T.);
#5670=ORIENTED_EDGE('',*,*,#4030,.T.);
#5671=ORIENTED_EDGE('',*,*,#4026,.F.);
#5672=ORIENTED_EDGE('',*,*,#4031,.T.);
#5673=ORIENTED_EDGE('',*,*,#4032,.T.);
#5674=ORIENTED_EDGE('',*,*,#4033,.T.);
#5675=ORIENTED_EDGE('',*,*,#4029,.F.);
#5676=ORIENTED_EDGE('',*,*,#4034,.T.);
#5677=ORIENTED_EDGE('',*,*,#4015,.F.);
#5678=ORIENTED_EDGE('',*,*,#4035,.T.);
#5679=ORIENTED_EDGE('',*,*,#4032,.F.);
#5680=ORIENTED_EDGE('',*,*,#4036,.T.);
#5681=ORIENTED_EDGE('',*,*,#4030,.F.);
#5682=ORIENTED_EDGE('',*,*,#4037,.F.);
#5683=ORIENTED_EDGE('',*,*,#4038,.F.);
#5684=ORIENTED_EDGE('',*,*,#4039,.F.);
#5685=ORIENTED_EDGE('',*,*,#4033,.F.);
#5686=ORIENTED_EDGE('',*,*,#4040,.T.);
#5687=ORIENTED_EDGE('',*,*,#4041,.T.);
#5688=ORIENTED_EDGE('',*,*,#4037,.T.);
#5689=ORIENTED_EDGE('',*,*,#4035,.F.);
#5690=ORIENTED_EDGE('',*,*,#4042,.F.);
#5691=ORIENTED_EDGE('',*,*,#4043,.F.);
#5692=ORIENTED_EDGE('',*,*,#4040,.F.);
#5693=ORIENTED_EDGE('',*,*,#4014,.F.);
#5694=ORIENTED_EDGE('',*,*,#4044,.T.);
#5695=ORIENTED_EDGE('',*,*,#4045,.T.);
#5696=ORIENTED_EDGE('',*,*,#4042,.T.);
#5697=ORIENTED_EDGE('',*,*,#4016,.F.);
#5698=ORIENTED_EDGE('',*,*,#4036,.F.);
#5699=ORIENTED_EDGE('',*,*,#4034,.F.);
#5700=ORIENTED_EDGE('',*,*,#4031,.F.);
#5701=ORIENTED_EDGE('',*,*,#4028,.F.);
#5702=ORIENTED_EDGE('',*,*,#4025,.F.);
#5703=ORIENTED_EDGE('',*,*,#4022,.F.);
#5704=ORIENTED_EDGE('',*,*,#4019,.F.);
#5705=ORIENTED_EDGE('',*,*,#3983,.T.);
#5706=ORIENTED_EDGE('',*,*,#3986,.T.);
#5707=ORIENTED_EDGE('',*,*,#4018,.F.);
#5708=ORIENTED_EDGE('',*,*,#4046,.F.);
#5709=ORIENTED_EDGE('',*,*,#4047,.F.);
#5710=ORIENTED_EDGE('',*,*,#4044,.F.);
#5711=ORIENTED_EDGE('',*,*,#4027,.F.);
#5712=ORIENTED_EDGE('',*,*,#4039,.T.);
#5713=ORIENTED_EDGE('',*,*,#4048,.T.);
#5714=ORIENTED_EDGE('',*,*,#4049,.T.);
#5715=ORIENTED_EDGE('',*,*,#4021,.F.);
#5716=ORIENTED_EDGE('',*,*,#4050,.T.);
#5717=ORIENTED_EDGE('',*,*,#4051,.T.);
#5718=ORIENTED_EDGE('',*,*,#4046,.T.);
#5719=ORIENTED_EDGE('',*,*,#4045,.F.);
#5720=ORIENTED_EDGE('',*,*,#4047,.T.);
#5721=ORIENTED_EDGE('',*,*,#4051,.F.);
#5722=ORIENTED_EDGE('',*,*,#4052,.T.);
#5723=ORIENTED_EDGE('',*,*,#4048,.F.);
#5724=ORIENTED_EDGE('',*,*,#4038,.T.);
#5725=ORIENTED_EDGE('',*,*,#4041,.F.);
#5726=ORIENTED_EDGE('',*,*,#4043,.T.);
#5727=ORIENTED_EDGE('',*,*,#3985,.T.);
#5728=ORIENTED_EDGE('',*,*,#3988,.T.);
#5729=ORIENTED_EDGE('',*,*,#4006,.T.);
#5730=ORIENTED_EDGE('',*,*,#4008,.T.);
#5731=ORIENTED_EDGE('',*,*,#4010,.T.);
#5732=ORIENTED_EDGE('',*,*,#4012,.T.);
#5733=ORIENTED_EDGE('',*,*,#4024,.F.);
#5734=ORIENTED_EDGE('',*,*,#4049,.F.);
#5735=ORIENTED_EDGE('',*,*,#4052,.F.);
#5736=ORIENTED_EDGE('',*,*,#4050,.F.);
#5737=ORIENTED_EDGE('',*,*,#4053,.F.);
#5738=ORIENTED_EDGE('',*,*,#4054,.T.);
#5739=ORIENTED_EDGE('',*,*,#4055,.T.);
#5740=ORIENTED_EDGE('',*,*,#4056,.T.);
#5741=ORIENTED_EDGE('',*,*,#4057,.F.);
#5742=ORIENTED_EDGE('',*,*,#4058,.T.);
#5743=ORIENTED_EDGE('',*,*,#4053,.T.);
#5744=ORIENTED_EDGE('',*,*,#4059,.T.);
#5745=ORIENTED_EDGE('',*,*,#4060,.F.);
#5746=ORIENTED_EDGE('',*,*,#4061,.T.);
#5747=ORIENTED_EDGE('',*,*,#4057,.T.);
#5748=ORIENTED_EDGE('',*,*,#4062,.T.);
#5749=ORIENTED_EDGE('',*,*,#4063,.F.);
#5750=ORIENTED_EDGE('',*,*,#4064,.T.);
#5751=ORIENTED_EDGE('',*,*,#4060,.T.);
#5752=ORIENTED_EDGE('',*,*,#4065,.T.);
#5753=ORIENTED_EDGE('',*,*,#4066,.F.);
#5754=ORIENTED_EDGE('',*,*,#4067,.T.);
#5755=ORIENTED_EDGE('',*,*,#4063,.T.);
#5756=ORIENTED_EDGE('',*,*,#4068,.T.);
#5757=ORIENTED_EDGE('',*,*,#4069,.F.);
#5758=ORIENTED_EDGE('',*,*,#4070,.T.);
#5759=ORIENTED_EDGE('',*,*,#4066,.T.);
#5760=ORIENTED_EDGE('',*,*,#4071,.T.);
#5761=ORIENTED_EDGE('',*,*,#4072,.F.);
#5762=ORIENTED_EDGE('',*,*,#4073,.T.);
#5763=ORIENTED_EDGE('',*,*,#4069,.T.);
#5764=ORIENTED_EDGE('',*,*,#4074,.T.);
#5765=ORIENTED_EDGE('',*,*,#4075,.F.);
#5766=ORIENTED_EDGE('',*,*,#4076,.T.);
#5767=ORIENTED_EDGE('',*,*,#4072,.T.);
#5768=ORIENTED_EDGE('',*,*,#4077,.T.);
#5769=ORIENTED_EDGE('',*,*,#4078,.F.);
#5770=ORIENTED_EDGE('',*,*,#4079,.T.);
#5771=ORIENTED_EDGE('',*,*,#4075,.T.);
#5772=ORIENTED_EDGE('',*,*,#4080,.T.);
#5773=ORIENTED_EDGE('',*,*,#4081,.F.);
#5774=ORIENTED_EDGE('',*,*,#4082,.T.);
#5775=ORIENTED_EDGE('',*,*,#4078,.T.);
#5776=ORIENTED_EDGE('',*,*,#4083,.T.);
#5777=ORIENTED_EDGE('',*,*,#4084,.F.);
#5778=ORIENTED_EDGE('',*,*,#4085,.T.);
#5779=ORIENTED_EDGE('',*,*,#4081,.T.);
#5780=ORIENTED_EDGE('',*,*,#4086,.T.);
#5781=ORIENTED_EDGE('',*,*,#4087,.F.);
#5782=ORIENTED_EDGE('',*,*,#4088,.T.);
#5783=ORIENTED_EDGE('',*,*,#4084,.T.);
#5784=ORIENTED_EDGE('',*,*,#4089,.T.);
#5785=ORIENTED_EDGE('',*,*,#4090,.F.);
#5786=ORIENTED_EDGE('',*,*,#4091,.T.);
#5787=ORIENTED_EDGE('',*,*,#4087,.T.);
#5788=ORIENTED_EDGE('',*,*,#4092,.T.);
#5789=ORIENTED_EDGE('',*,*,#4093,.F.);
#5790=ORIENTED_EDGE('',*,*,#4094,.T.);
#5791=ORIENTED_EDGE('',*,*,#4090,.T.);
#5792=ORIENTED_EDGE('',*,*,#4095,.T.);
#5793=ORIENTED_EDGE('',*,*,#4096,.F.);
#5794=ORIENTED_EDGE('',*,*,#4097,.T.);
#5795=ORIENTED_EDGE('',*,*,#4093,.T.);
#5796=ORIENTED_EDGE('',*,*,#4098,.T.);
#5797=ORIENTED_EDGE('',*,*,#4099,.F.);
#5798=ORIENTED_EDGE('',*,*,#4100,.T.);
#5799=ORIENTED_EDGE('',*,*,#4096,.T.);
#5800=ORIENTED_EDGE('',*,*,#4101,.T.);
#5801=ORIENTED_EDGE('',*,*,#4102,.F.);
#5802=ORIENTED_EDGE('',*,*,#4103,.T.);
#5803=ORIENTED_EDGE('',*,*,#4099,.T.);
#5804=ORIENTED_EDGE('',*,*,#4104,.T.);
#5805=ORIENTED_EDGE('',*,*,#4105,.F.);
#5806=ORIENTED_EDGE('',*,*,#4106,.T.);
#5807=ORIENTED_EDGE('',*,*,#4102,.T.);
#5808=ORIENTED_EDGE('',*,*,#4107,.T.);
#5809=ORIENTED_EDGE('',*,*,#4108,.F.);
#5810=ORIENTED_EDGE('',*,*,#4109,.T.);
#5811=ORIENTED_EDGE('',*,*,#4105,.T.);
#5812=ORIENTED_EDGE('',*,*,#4110,.T.);
#5813=ORIENTED_EDGE('',*,*,#4111,.F.);
#5814=ORIENTED_EDGE('',*,*,#4112,.T.);
#5815=ORIENTED_EDGE('',*,*,#4108,.T.);
#5816=ORIENTED_EDGE('',*,*,#4113,.T.);
#5817=ORIENTED_EDGE('',*,*,#4114,.F.);
#5818=ORIENTED_EDGE('',*,*,#4115,.T.);
#5819=ORIENTED_EDGE('',*,*,#4111,.T.);
#5820=ORIENTED_EDGE('',*,*,#4116,.T.);
#5821=ORIENTED_EDGE('',*,*,#4117,.F.);
#5822=ORIENTED_EDGE('',*,*,#4118,.T.);
#5823=ORIENTED_EDGE('',*,*,#4114,.T.);
#5824=ORIENTED_EDGE('',*,*,#4119,.T.);
#5825=ORIENTED_EDGE('',*,*,#4120,.F.);
#5826=ORIENTED_EDGE('',*,*,#4121,.T.);
#5827=ORIENTED_EDGE('',*,*,#4117,.T.);
#5828=ORIENTED_EDGE('',*,*,#4122,.T.);
#5829=ORIENTED_EDGE('',*,*,#4123,.F.);
#5830=ORIENTED_EDGE('',*,*,#4124,.T.);
#5831=ORIENTED_EDGE('',*,*,#4120,.T.);
#5832=ORIENTED_EDGE('',*,*,#4125,.T.);
#5833=ORIENTED_EDGE('',*,*,#4126,.F.);
#5834=ORIENTED_EDGE('',*,*,#4127,.T.);
#5835=ORIENTED_EDGE('',*,*,#4123,.T.);
#5836=ORIENTED_EDGE('',*,*,#4128,.T.);
#5837=ORIENTED_EDGE('',*,*,#4129,.F.);
#5838=ORIENTED_EDGE('',*,*,#4130,.T.);
#5839=ORIENTED_EDGE('',*,*,#4126,.T.);
#5840=ORIENTED_EDGE('',*,*,#4131,.T.);
#5841=ORIENTED_EDGE('',*,*,#4132,.F.);
#5842=ORIENTED_EDGE('',*,*,#4133,.T.);
#5843=ORIENTED_EDGE('',*,*,#4129,.T.);
#5844=ORIENTED_EDGE('',*,*,#4134,.T.);
#5845=ORIENTED_EDGE('',*,*,#4135,.F.);
#5846=ORIENTED_EDGE('',*,*,#4136,.T.);
#5847=ORIENTED_EDGE('',*,*,#4132,.T.);
#5848=ORIENTED_EDGE('',*,*,#4137,.T.);
#5849=ORIENTED_EDGE('',*,*,#4138,.F.);
#5850=ORIENTED_EDGE('',*,*,#4139,.T.);
#5851=ORIENTED_EDGE('',*,*,#4135,.T.);
#5852=ORIENTED_EDGE('',*,*,#4140,.T.);
#5853=ORIENTED_EDGE('',*,*,#4141,.F.);
#5854=ORIENTED_EDGE('',*,*,#4142,.T.);
#5855=ORIENTED_EDGE('',*,*,#4138,.T.);
#5856=ORIENTED_EDGE('',*,*,#4143,.T.);
#5857=ORIENTED_EDGE('',*,*,#4144,.F.);
#5858=ORIENTED_EDGE('',*,*,#4145,.T.);
#5859=ORIENTED_EDGE('',*,*,#4146,.T.);
#5860=ORIENTED_EDGE('',*,*,#4147,.F.);
#5861=ORIENTED_EDGE('',*,*,#4148,.F.);
#5862=ORIENTED_EDGE('',*,*,#4149,.T.);
#5863=ORIENTED_EDGE('',*,*,#4144,.T.);
#5864=ORIENTED_EDGE('',*,*,#4150,.F.);
#5865=ORIENTED_EDGE('',*,*,#4151,.F.);
#5866=ORIENTED_EDGE('',*,*,#4152,.T.);
#5867=ORIENTED_EDGE('',*,*,#4148,.T.);
#5868=ORIENTED_EDGE('',*,*,#4153,.F.);
#5869=ORIENTED_EDGE('',*,*,#4154,.F.);
#5870=ORIENTED_EDGE('',*,*,#4155,.T.);
#5871=ORIENTED_EDGE('',*,*,#4151,.T.);
#5872=ORIENTED_EDGE('',*,*,#4156,.F.);
#5873=ORIENTED_EDGE('',*,*,#4157,.F.);
#5874=ORIENTED_EDGE('',*,*,#4158,.T.);
#5875=ORIENTED_EDGE('',*,*,#4154,.T.);
#5876=ORIENTED_EDGE('',*,*,#4159,.F.);
#5877=ORIENTED_EDGE('',*,*,#4160,.F.);
#5878=ORIENTED_EDGE('',*,*,#4161,.T.);
#5879=ORIENTED_EDGE('',*,*,#4157,.T.);
#5880=ORIENTED_EDGE('',*,*,#4162,.F.);
#5881=ORIENTED_EDGE('',*,*,#4163,.F.);
#5882=ORIENTED_EDGE('',*,*,#4164,.T.);
#5883=ORIENTED_EDGE('',*,*,#4160,.T.);
#5884=ORIENTED_EDGE('',*,*,#4165,.F.);
#5885=ORIENTED_EDGE('',*,*,#4166,.F.);
#5886=ORIENTED_EDGE('',*,*,#4167,.T.);
#5887=ORIENTED_EDGE('',*,*,#4163,.T.);
#5888=ORIENTED_EDGE('',*,*,#4168,.F.);
#5889=ORIENTED_EDGE('',*,*,#4169,.F.);
#5890=ORIENTED_EDGE('',*,*,#4170,.T.);
#5891=ORIENTED_EDGE('',*,*,#4166,.T.);
#5892=ORIENTED_EDGE('',*,*,#4171,.F.);
#5893=ORIENTED_EDGE('',*,*,#4172,.F.);
#5894=ORIENTED_EDGE('',*,*,#4173,.T.);
#5895=ORIENTED_EDGE('',*,*,#4169,.T.);
#5896=ORIENTED_EDGE('',*,*,#4174,.F.);
#5897=ORIENTED_EDGE('',*,*,#4175,.F.);
#5898=ORIENTED_EDGE('',*,*,#4176,.T.);
#5899=ORIENTED_EDGE('',*,*,#4172,.T.);
#5900=ORIENTED_EDGE('',*,*,#4177,.F.);
#5901=ORIENTED_EDGE('',*,*,#4178,.F.);
#5902=ORIENTED_EDGE('',*,*,#4179,.T.);
#5903=ORIENTED_EDGE('',*,*,#4175,.T.);
#5904=ORIENTED_EDGE('',*,*,#4180,.F.);
#5905=ORIENTED_EDGE('',*,*,#4181,.F.);
#5906=ORIENTED_EDGE('',*,*,#4182,.T.);
#5907=ORIENTED_EDGE('',*,*,#4178,.T.);
#5908=ORIENTED_EDGE('',*,*,#4183,.F.);
#5909=ORIENTED_EDGE('',*,*,#4184,.F.);
#5910=ORIENTED_EDGE('',*,*,#4185,.T.);
#5911=ORIENTED_EDGE('',*,*,#4181,.T.);
#5912=ORIENTED_EDGE('',*,*,#4186,.F.);
#5913=ORIENTED_EDGE('',*,*,#4187,.F.);
#5914=ORIENTED_EDGE('',*,*,#4188,.T.);
#5915=ORIENTED_EDGE('',*,*,#4184,.T.);
#5916=ORIENTED_EDGE('',*,*,#4189,.F.);
#5917=ORIENTED_EDGE('',*,*,#4190,.F.);
#5918=ORIENTED_EDGE('',*,*,#4191,.T.);
#5919=ORIENTED_EDGE('',*,*,#4187,.T.);
#5920=ORIENTED_EDGE('',*,*,#4192,.F.);
#5921=ORIENTED_EDGE('',*,*,#4193,.F.);
#5922=ORIENTED_EDGE('',*,*,#4194,.T.);
#5923=ORIENTED_EDGE('',*,*,#4190,.T.);
#5924=ORIENTED_EDGE('',*,*,#4195,.F.);
#5925=ORIENTED_EDGE('',*,*,#4196,.F.);
#5926=ORIENTED_EDGE('',*,*,#4197,.T.);
#5927=ORIENTED_EDGE('',*,*,#4193,.T.);
#5928=ORIENTED_EDGE('',*,*,#4198,.F.);
#5929=ORIENTED_EDGE('',*,*,#4199,.F.);
#5930=ORIENTED_EDGE('',*,*,#4200,.T.);
#5931=ORIENTED_EDGE('',*,*,#4196,.T.);
#5932=ORIENTED_EDGE('',*,*,#4201,.F.);
#5933=ORIENTED_EDGE('',*,*,#4202,.F.);
#5934=ORIENTED_EDGE('',*,*,#4203,.T.);
#5935=ORIENTED_EDGE('',*,*,#4199,.T.);
#5936=ORIENTED_EDGE('',*,*,#4204,.F.);
#5937=ORIENTED_EDGE('',*,*,#4205,.F.);
#5938=ORIENTED_EDGE('',*,*,#4206,.T.);
#5939=ORIENTED_EDGE('',*,*,#4202,.T.);
#5940=ORIENTED_EDGE('',*,*,#4207,.F.);
#5941=ORIENTED_EDGE('',*,*,#4208,.F.);
#5942=ORIENTED_EDGE('',*,*,#4209,.T.);
#5943=ORIENTED_EDGE('',*,*,#4205,.T.);
#5944=ORIENTED_EDGE('',*,*,#4210,.F.);
#5945=ORIENTED_EDGE('',*,*,#4211,.F.);
#5946=ORIENTED_EDGE('',*,*,#4212,.T.);
#5947=ORIENTED_EDGE('',*,*,#4208,.T.);
#5948=ORIENTED_EDGE('',*,*,#4213,.F.);
#5949=ORIENTED_EDGE('',*,*,#4214,.F.);
#5950=ORIENTED_EDGE('',*,*,#4215,.T.);
#5951=ORIENTED_EDGE('',*,*,#4211,.T.);
#5952=ORIENTED_EDGE('',*,*,#4216,.F.);
#5953=ORIENTED_EDGE('',*,*,#4217,.F.);
#5954=ORIENTED_EDGE('',*,*,#4218,.T.);
#5955=ORIENTED_EDGE('',*,*,#4214,.T.);
#5956=ORIENTED_EDGE('',*,*,#4219,.F.);
#5957=ORIENTED_EDGE('',*,*,#4220,.F.);
#5958=ORIENTED_EDGE('',*,*,#4221,.T.);
#5959=ORIENTED_EDGE('',*,*,#4217,.T.);
#5960=ORIENTED_EDGE('',*,*,#4222,.F.);
#5961=ORIENTED_EDGE('',*,*,#4223,.F.);
#5962=ORIENTED_EDGE('',*,*,#4224,.T.);
#5963=ORIENTED_EDGE('',*,*,#4220,.T.);
#5964=ORIENTED_EDGE('',*,*,#4225,.F.);
#5965=ORIENTED_EDGE('',*,*,#4226,.F.);
#5966=ORIENTED_EDGE('',*,*,#4227,.T.);
#5967=ORIENTED_EDGE('',*,*,#4223,.T.);
#5968=ORIENTED_EDGE('',*,*,#4228,.F.);
#5969=ORIENTED_EDGE('',*,*,#4229,.F.);
#5970=ORIENTED_EDGE('',*,*,#4230,.T.);
#5971=ORIENTED_EDGE('',*,*,#4226,.T.);
#5972=ORIENTED_EDGE('',*,*,#4231,.F.);
#5973=ORIENTED_EDGE('',*,*,#4232,.F.);
#5974=ORIENTED_EDGE('',*,*,#4233,.T.);
#5975=ORIENTED_EDGE('',*,*,#4229,.T.);
#5976=ORIENTED_EDGE('',*,*,#4234,.F.);
#5977=ORIENTED_EDGE('',*,*,#4235,.F.);
#5978=ORIENTED_EDGE('',*,*,#4146,.F.);
#5979=ORIENTED_EDGE('',*,*,#4236,.F.);
#5980=ORIENTED_EDGE('',*,*,#4237,.F.);
#5981=ORIENTED_EDGE('',*,*,#4238,.F.);
#5982=ORIENTED_EDGE('',*,*,#4239,.T.);
#5983=ORIENTED_EDGE('',*,*,#4240,.F.);
#5984=ORIENTED_EDGE('',*,*,#4239,.F.);
#5985=ORIENTED_EDGE('',*,*,#4236,.T.);
#5986=ORIENTED_EDGE('',*,*,#4145,.F.);
#5987=ORIENTED_EDGE('',*,*,#4149,.F.);
#5988=ORIENTED_EDGE('',*,*,#4152,.F.);
#5989=ORIENTED_EDGE('',*,*,#4155,.F.);
#5990=ORIENTED_EDGE('',*,*,#4158,.F.);
#5991=ORIENTED_EDGE('',*,*,#4161,.F.);
#5992=ORIENTED_EDGE('',*,*,#4164,.F.);
#5993=ORIENTED_EDGE('',*,*,#4167,.F.);
#5994=ORIENTED_EDGE('',*,*,#4170,.F.);
#5995=ORIENTED_EDGE('',*,*,#4173,.F.);
#5996=ORIENTED_EDGE('',*,*,#4176,.F.);
#5997=ORIENTED_EDGE('',*,*,#4179,.F.);
#5998=ORIENTED_EDGE('',*,*,#4182,.F.);
#5999=ORIENTED_EDGE('',*,*,#4185,.F.);
#6000=ORIENTED_EDGE('',*,*,#4188,.F.);
#6001=ORIENTED_EDGE('',*,*,#4191,.F.);
#6002=ORIENTED_EDGE('',*,*,#4194,.F.);
#6003=ORIENTED_EDGE('',*,*,#4197,.F.);
#6004=ORIENTED_EDGE('',*,*,#4200,.F.);
#6005=ORIENTED_EDGE('',*,*,#4203,.F.);
#6006=ORIENTED_EDGE('',*,*,#4206,.F.);
#6007=ORIENTED_EDGE('',*,*,#4209,.F.);
#6008=ORIENTED_EDGE('',*,*,#4212,.F.);
#6009=ORIENTED_EDGE('',*,*,#4215,.F.);
#6010=ORIENTED_EDGE('',*,*,#4218,.F.);
#6011=ORIENTED_EDGE('',*,*,#4221,.F.);
#6012=ORIENTED_EDGE('',*,*,#4224,.F.);
#6013=ORIENTED_EDGE('',*,*,#4227,.F.);
#6014=ORIENTED_EDGE('',*,*,#4230,.F.);
#6015=ORIENTED_EDGE('',*,*,#4233,.F.);
#6016=ORIENTED_EDGE('',*,*,#4241,.F.);
#6017=ORIENTED_EDGE('',*,*,#4242,.F.);
#6018=ORIENTED_EDGE('',*,*,#4054,.F.);
#6019=ORIENTED_EDGE('',*,*,#4058,.F.);
#6020=ORIENTED_EDGE('',*,*,#4061,.F.);
#6021=ORIENTED_EDGE('',*,*,#4064,.F.);
#6022=ORIENTED_EDGE('',*,*,#4067,.F.);
#6023=ORIENTED_EDGE('',*,*,#4070,.F.);
#6024=ORIENTED_EDGE('',*,*,#4073,.F.);
#6025=ORIENTED_EDGE('',*,*,#4076,.F.);
#6026=ORIENTED_EDGE('',*,*,#4079,.F.);
#6027=ORIENTED_EDGE('',*,*,#4082,.F.);
#6028=ORIENTED_EDGE('',*,*,#4085,.F.);
#6029=ORIENTED_EDGE('',*,*,#4088,.F.);
#6030=ORIENTED_EDGE('',*,*,#4091,.F.);
#6031=ORIENTED_EDGE('',*,*,#4094,.F.);
#6032=ORIENTED_EDGE('',*,*,#4097,.F.);
#6033=ORIENTED_EDGE('',*,*,#4100,.F.);
#6034=ORIENTED_EDGE('',*,*,#4103,.F.);
#6035=ORIENTED_EDGE('',*,*,#4106,.F.);
#6036=ORIENTED_EDGE('',*,*,#4109,.F.);
#6037=ORIENTED_EDGE('',*,*,#4112,.F.);
#6038=ORIENTED_EDGE('',*,*,#4115,.F.);
#6039=ORIENTED_EDGE('',*,*,#4118,.F.);
#6040=ORIENTED_EDGE('',*,*,#4121,.F.);
#6041=ORIENTED_EDGE('',*,*,#4124,.F.);
#6042=ORIENTED_EDGE('',*,*,#4127,.F.);
#6043=ORIENTED_EDGE('',*,*,#4130,.F.);
#6044=ORIENTED_EDGE('',*,*,#4133,.F.);
#6045=ORIENTED_EDGE('',*,*,#4136,.F.);
#6046=ORIENTED_EDGE('',*,*,#4139,.F.);
#6047=ORIENTED_EDGE('',*,*,#4142,.F.);
#6048=ORIENTED_EDGE('',*,*,#4243,.F.);
#6049=ORIENTED_EDGE('',*,*,#4232,.T.);
#6050=ORIENTED_EDGE('',*,*,#4244,.F.);
#6051=ORIENTED_EDGE('',*,*,#4245,.F.);
#6052=ORIENTED_EDGE('',*,*,#4241,.T.);
#6053=ORIENTED_EDGE('',*,*,#4235,.T.);
#6054=ORIENTED_EDGE('',*,*,#4238,.T.);
#6055=ORIENTED_EDGE('',*,*,#4246,.F.);
#6056=ORIENTED_EDGE('',*,*,#4143,.F.);
#6057=ORIENTED_EDGE('',*,*,#4140,.F.);
#6058=ORIENTED_EDGE('',*,*,#4137,.F.);
#6059=ORIENTED_EDGE('',*,*,#4134,.F.);
#6060=ORIENTED_EDGE('',*,*,#4131,.F.);
#6061=ORIENTED_EDGE('',*,*,#4128,.F.);
#6062=ORIENTED_EDGE('',*,*,#4125,.F.);
#6063=ORIENTED_EDGE('',*,*,#4122,.F.);
#6064=ORIENTED_EDGE('',*,*,#4119,.F.);
#6065=ORIENTED_EDGE('',*,*,#4116,.F.);
#6066=ORIENTED_EDGE('',*,*,#4113,.F.);
#6067=ORIENTED_EDGE('',*,*,#4110,.F.);
#6068=ORIENTED_EDGE('',*,*,#4107,.F.);
#6069=ORIENTED_EDGE('',*,*,#4104,.F.);
#6070=ORIENTED_EDGE('',*,*,#4101,.F.);
#6071=ORIENTED_EDGE('',*,*,#4098,.F.);
#6072=ORIENTED_EDGE('',*,*,#4095,.F.);
#6073=ORIENTED_EDGE('',*,*,#4092,.F.);
#6074=ORIENTED_EDGE('',*,*,#4089,.F.);
#6075=ORIENTED_EDGE('',*,*,#4086,.F.);
#6076=ORIENTED_EDGE('',*,*,#4083,.F.);
#6077=ORIENTED_EDGE('',*,*,#4080,.F.);
#6078=ORIENTED_EDGE('',*,*,#4077,.F.);
#6079=ORIENTED_EDGE('',*,*,#4074,.F.);
#6080=ORIENTED_EDGE('',*,*,#4071,.F.);
#6081=ORIENTED_EDGE('',*,*,#4068,.F.);
#6082=ORIENTED_EDGE('',*,*,#4065,.F.);
#6083=ORIENTED_EDGE('',*,*,#4062,.F.);
#6084=ORIENTED_EDGE('',*,*,#4059,.F.);
#6085=ORIENTED_EDGE('',*,*,#4056,.F.);
#6086=ORIENTED_EDGE('',*,*,#4247,.F.);
#6087=ORIENTED_EDGE('',*,*,#4244,.T.);
#6088=ORIENTED_EDGE('',*,*,#4234,.T.);
#6089=ORIENTED_EDGE('',*,*,#4231,.T.);
#6090=ORIENTED_EDGE('',*,*,#4228,.T.);
#6091=ORIENTED_EDGE('',*,*,#4225,.T.);
#6092=ORIENTED_EDGE('',*,*,#4222,.T.);
#6093=ORIENTED_EDGE('',*,*,#4219,.T.);
#6094=ORIENTED_EDGE('',*,*,#4216,.T.);
#6095=ORIENTED_EDGE('',*,*,#4213,.T.);
#6096=ORIENTED_EDGE('',*,*,#4210,.T.);
#6097=ORIENTED_EDGE('',*,*,#4207,.T.);
#6098=ORIENTED_EDGE('',*,*,#4204,.T.);
#6099=ORIENTED_EDGE('',*,*,#4201,.T.);
#6100=ORIENTED_EDGE('',*,*,#4198,.T.);
#6101=ORIENTED_EDGE('',*,*,#4195,.T.);
#6102=ORIENTED_EDGE('',*,*,#4192,.T.);
#6103=ORIENTED_EDGE('',*,*,#4189,.T.);
#6104=ORIENTED_EDGE('',*,*,#4186,.T.);
#6105=ORIENTED_EDGE('',*,*,#4183,.T.);
#6106=ORIENTED_EDGE('',*,*,#4180,.T.);
#6107=ORIENTED_EDGE('',*,*,#4177,.T.);
#6108=ORIENTED_EDGE('',*,*,#4174,.T.);
#6109=ORIENTED_EDGE('',*,*,#4171,.T.);
#6110=ORIENTED_EDGE('',*,*,#4168,.T.);
#6111=ORIENTED_EDGE('',*,*,#4165,.T.);
#6112=ORIENTED_EDGE('',*,*,#4162,.T.);
#6113=ORIENTED_EDGE('',*,*,#4159,.T.);
#6114=ORIENTED_EDGE('',*,*,#4156,.T.);
#6115=ORIENTED_EDGE('',*,*,#4153,.T.);
#6116=ORIENTED_EDGE('',*,*,#4150,.T.);
#6117=ORIENTED_EDGE('',*,*,#4147,.T.);
#6118=ORIENTED_EDGE('',*,*,#4141,.T.);
#6119=ORIENTED_EDGE('',*,*,#4246,.T.);
#6120=ORIENTED_EDGE('',*,*,#4237,.T.);
#6121=ORIENTED_EDGE('',*,*,#4243,.T.);
#6122=ORIENTED_EDGE('',*,*,#4248,.F.);
#6123=ORIENTED_EDGE('',*,*,#4249,.T.);
#6124=ORIENTED_EDGE('',*,*,#4250,.T.);
#6125=ORIENTED_EDGE('',*,*,#4251,.F.);
#6126=ORIENTED_EDGE('',*,*,#4252,.F.);
#6127=ORIENTED_EDGE('',*,*,#4253,.T.);
#6128=ORIENTED_EDGE('',*,*,#4254,.T.);
#6129=ORIENTED_EDGE('',*,*,#4249,.F.);
#6130=ORIENTED_EDGE('',*,*,#4255,.F.);
#6131=ORIENTED_EDGE('',*,*,#4256,.T.);
#6132=ORIENTED_EDGE('',*,*,#4257,.T.);
#6133=ORIENTED_EDGE('',*,*,#4253,.F.);
#6134=ORIENTED_EDGE('',*,*,#4258,.F.);
#6135=ORIENTED_EDGE('',*,*,#4259,.T.);
#6136=ORIENTED_EDGE('',*,*,#4260,.T.);
#6137=ORIENTED_EDGE('',*,*,#4256,.F.);
#6138=ORIENTED_EDGE('',*,*,#4261,.F.);
#6139=ORIENTED_EDGE('',*,*,#4262,.T.);
#6140=ORIENTED_EDGE('',*,*,#4263,.T.);
#6141=ORIENTED_EDGE('',*,*,#4259,.F.);
#6142=ORIENTED_EDGE('',*,*,#4264,.F.);
#6143=ORIENTED_EDGE('',*,*,#4251,.T.);
#6144=ORIENTED_EDGE('',*,*,#4265,.T.);
#6145=ORIENTED_EDGE('',*,*,#4262,.F.);
#6146=ORIENTED_EDGE('',*,*,#4265,.F.);
#6147=ORIENTED_EDGE('',*,*,#4250,.F.);
#6148=ORIENTED_EDGE('',*,*,#4254,.F.);
#6149=ORIENTED_EDGE('',*,*,#4257,.F.);
#6150=ORIENTED_EDGE('',*,*,#4260,.F.);
#6151=ORIENTED_EDGE('',*,*,#4263,.F.);
#6152=ORIENTED_EDGE('',*,*,#4266,.T.);
#6153=ORIENTED_EDGE('',*,*,#4242,.T.);
#6154=ORIENTED_EDGE('',*,*,#4245,.T.);
#6155=ORIENTED_EDGE('',*,*,#4247,.T.);
#6156=ORIENTED_EDGE('',*,*,#4055,.F.);
#6157=ORIENTED_EDGE('',*,*,#4266,.F.);
#6158=ORIENTED_EDGE('',*,*,#4267,.T.);
#6159=ORIENTED_EDGE('',*,*,#4268,.T.);
#6160=ORIENTED_EDGE('',*,*,#4267,.F.);
#6161=ORIENTED_EDGE('',*,*,#4268,.F.);
#6162=ORIENTED_EDGE('',*,*,#4248,.T.);
#6163=ORIENTED_EDGE('',*,*,#4264,.T.);
#6164=ORIENTED_EDGE('',*,*,#4261,.T.);
#6165=ORIENTED_EDGE('',*,*,#4258,.T.);
#6166=ORIENTED_EDGE('',*,*,#4255,.T.);
#6167=ORIENTED_EDGE('',*,*,#4252,.T.);
#6168=ORIENTED_EDGE('',*,*,#4240,.T.);
#6169=ORIENTED_EDGE('',*,*,#4269,.T.);
#6170=ORIENTED_EDGE('',*,*,#4270,.F.);
#6171=ORIENTED_EDGE('',*,*,#4271,.T.);
#6172=ORIENTED_EDGE('',*,*,#4272,.T.);
#6173=ORIENTED_EDGE('',*,*,#4273,.T.);
#6174=ORIENTED_EDGE('',*,*,#4274,.F.);
#6175=ORIENTED_EDGE('',*,*,#4269,.F.);
#6176=ORIENTED_EDGE('',*,*,#4275,.T.);
#6177=ORIENTED_EDGE('',*,*,#4276,.T.);
#6178=ORIENTED_EDGE('',*,*,#4277,.T.);
#6179=ORIENTED_EDGE('',*,*,#4272,.F.);
#6180=ORIENTED_EDGE('',*,*,#4278,.T.);
#6181=ORIENTED_EDGE('',*,*,#4279,.T.);
#6182=ORIENTED_EDGE('',*,*,#4280,.T.);
#6183=ORIENTED_EDGE('',*,*,#4276,.F.);
#6184=ORIENTED_EDGE('',*,*,#4281,.T.);
#6185=ORIENTED_EDGE('',*,*,#4282,.F.);
#6186=ORIENTED_EDGE('',*,*,#4283,.T.);
#6187=ORIENTED_EDGE('',*,*,#4284,.F.);
#6188=ORIENTED_EDGE('',*,*,#4285,.T.);
#6189=ORIENTED_EDGE('',*,*,#4286,.T.);
#6190=ORIENTED_EDGE('',*,*,#4287,.T.);
#6191=ORIENTED_EDGE('',*,*,#4288,.F.);
#6192=ORIENTED_EDGE('',*,*,#4289,.F.);
#6193=ORIENTED_EDGE('',*,*,#4290,.T.);
#6194=ORIENTED_EDGE('',*,*,#4291,.T.);
#6195=ORIENTED_EDGE('',*,*,#4286,.F.);
#6196=ORIENTED_EDGE('',*,*,#4292,.F.);
#6197=ORIENTED_EDGE('',*,*,#4293,.T.);
#6198=ORIENTED_EDGE('',*,*,#4294,.T.);
#6199=ORIENTED_EDGE('',*,*,#4290,.F.);
#6200=ORIENTED_EDGE('',*,*,#4295,.F.);
#6201=ORIENTED_EDGE('',*,*,#4296,.T.);
#6202=ORIENTED_EDGE('',*,*,#4297,.T.);
#6203=ORIENTED_EDGE('',*,*,#4293,.F.);
#6204=ORIENTED_EDGE('',*,*,#4298,.F.);
#6205=ORIENTED_EDGE('',*,*,#4299,.F.);
#6206=ORIENTED_EDGE('',*,*,#4300,.F.);
#6207=ORIENTED_EDGE('',*,*,#4301,.F.);
#6208=ORIENTED_EDGE('',*,*,#4302,.T.);
#6209=ORIENTED_EDGE('',*,*,#4299,.T.);
#6210=ORIENTED_EDGE('',*,*,#4303,.T.);
#6211=ORIENTED_EDGE('',*,*,#4296,.F.);
#6212=ORIENTED_EDGE('',*,*,#4304,.F.);
#6213=ORIENTED_EDGE('',*,*,#4305,.F.);
#6214=ORIENTED_EDGE('',*,*,#4287,.F.);
#6215=ORIENTED_EDGE('',*,*,#4291,.F.);
#6216=ORIENTED_EDGE('',*,*,#4294,.F.);
#6217=ORIENTED_EDGE('',*,*,#4297,.F.);
#6218=ORIENTED_EDGE('',*,*,#4303,.F.);
#6219=ORIENTED_EDGE('',*,*,#4302,.F.);
#6220=ORIENTED_EDGE('',*,*,#4306,.F.);
#6221=ORIENTED_EDGE('',*,*,#4283,.F.);
#6222=ORIENTED_EDGE('',*,*,#4307,.F.);
#6223=ORIENTED_EDGE('',*,*,#4281,.F.);
#6224=ORIENTED_EDGE('',*,*,#4278,.F.);
#6225=ORIENTED_EDGE('',*,*,#4275,.F.);
#6226=ORIENTED_EDGE('',*,*,#4271,.F.);
#6227=ORIENTED_EDGE('',*,*,#4308,.F.);
#6228=ORIENTED_EDGE('',*,*,#4273,.F.);
#6229=ORIENTED_EDGE('',*,*,#4277,.F.);
#6230=ORIENTED_EDGE('',*,*,#4280,.F.);
#6231=ORIENTED_EDGE('',*,*,#4309,.F.);
#6232=ORIENTED_EDGE('',*,*,#4285,.F.);
#6233=ORIENTED_EDGE('',*,*,#4310,.F.);
#6234=ORIENTED_EDGE('',*,*,#4300,.T.);
#6235=ORIENTED_EDGE('',*,*,#4304,.T.);
#6236=ORIENTED_EDGE('',*,*,#4298,.T.);
#6237=ORIENTED_EDGE('',*,*,#4295,.T.);
#6238=ORIENTED_EDGE('',*,*,#4292,.T.);
#6239=ORIENTED_EDGE('',*,*,#4289,.T.);
#6240=ORIENTED_EDGE('',*,*,#4311,.T.);
#6241=ORIENTED_EDGE('',*,*,#4312,.T.);
#6242=ORIENTED_EDGE('',*,*,#4313,.T.);
#6243=ORIENTED_EDGE('',*,*,#4314,.T.);
#6244=ORIENTED_EDGE('',*,*,#4315,.T.);
#6245=ORIENTED_EDGE('',*,*,#4316,.T.);
#6246=ORIENTED_EDGE('',*,*,#4306,.T.);
#6247=ORIENTED_EDGE('',*,*,#4301,.T.);
#6248=ORIENTED_EDGE('',*,*,#4310,.T.);
#6249=ORIENTED_EDGE('',*,*,#4284,.T.);
#6250=ORIENTED_EDGE('',*,*,#4282,.T.);
#6251=ORIENTED_EDGE('',*,*,#4309,.T.);
#6252=ORIENTED_EDGE('',*,*,#4279,.F.);
#6253=ORIENTED_EDGE('',*,*,#4307,.T.);
#6254=ORIENTED_EDGE('',*,*,#4317,.T.);
#6255=ORIENTED_EDGE('',*,*,#4318,.T.);
#6256=ORIENTED_EDGE('',*,*,#4316,.F.);
#6257=ORIENTED_EDGE('',*,*,#4319,.F.);
#6258=ORIENTED_EDGE('',*,*,#4320,.T.);
#6259=ORIENTED_EDGE('',*,*,#4319,.T.);
#6260=ORIENTED_EDGE('',*,*,#4315,.F.);
#6261=ORIENTED_EDGE('',*,*,#4321,.F.);
#6262=ORIENTED_EDGE('',*,*,#4322,.T.);
#6263=ORIENTED_EDGE('',*,*,#4321,.T.);
#6264=ORIENTED_EDGE('',*,*,#4314,.F.);
#6265=ORIENTED_EDGE('',*,*,#4323,.F.);
#6266=ORIENTED_EDGE('',*,*,#4324,.T.);
#6267=ORIENTED_EDGE('',*,*,#4323,.T.);
#6268=ORIENTED_EDGE('',*,*,#4313,.F.);
#6269=ORIENTED_EDGE('',*,*,#4325,.F.);
#6270=ORIENTED_EDGE('',*,*,#4326,.T.);
#6271=ORIENTED_EDGE('',*,*,#4325,.T.);
#6272=ORIENTED_EDGE('',*,*,#4312,.F.);
#6273=ORIENTED_EDGE('',*,*,#4327,.F.);
#6274=ORIENTED_EDGE('',*,*,#4328,.T.);
#6275=ORIENTED_EDGE('',*,*,#4327,.T.);
#6276=ORIENTED_EDGE('',*,*,#4311,.F.);
#6277=ORIENTED_EDGE('',*,*,#4318,.F.);
#6278=ORIENTED_EDGE('',*,*,#4328,.F.);
#6279=ORIENTED_EDGE('',*,*,#4317,.F.);
#6280=ORIENTED_EDGE('',*,*,#4320,.F.);
#6281=ORIENTED_EDGE('',*,*,#4322,.F.);
#6282=ORIENTED_EDGE('',*,*,#4324,.F.);
#6283=ORIENTED_EDGE('',*,*,#4326,.F.);
#6284=ORIENTED_EDGE('',*,*,#4305,.T.);
#6285=ORIENTED_EDGE('',*,*,#4270,.T.);
#6286=ORIENTED_EDGE('',*,*,#4274,.T.);
#6287=ORIENTED_EDGE('',*,*,#4308,.T.);
#6288=ORIENTED_EDGE('',*,*,#4288,.T.);
#6289=ORIENTED_EDGE('',*,*,#4329,.F.);
#6290=ORIENTED_EDGE('',*,*,#4330,.T.);
#6291=ORIENTED_EDGE('',*,*,#4331,.T.);
#6292=ORIENTED_EDGE('',*,*,#4330,.F.);
#6293=ORIENTED_EDGE('',*,*,#4332,.F.);
#6294=ORIENTED_EDGE('',*,*,#4333,.T.);
#6295=ORIENTED_EDGE('',*,*,#4334,.T.);
#6296=ORIENTED_EDGE('',*,*,#4333,.F.);
#6297=ORIENTED_EDGE('',*,*,#4332,.T.);
#6298=ORIENTED_EDGE('',*,*,#4329,.T.);
#6299=ORIENTED_EDGE('',*,*,#4334,.F.);
#6300=ORIENTED_EDGE('',*,*,#4331,.F.);
#6301=CYLINDRICAL_SURFACE('',#6943,0.17);
#6302=CYLINDRICAL_SURFACE('',#6946,0.17);
#6303=CYLINDRICAL_SURFACE('',#6949,0.41);
#6304=CYLINDRICAL_SURFACE('',#6972,1.4);
#6305=CYLINDRICAL_SURFACE('',#6979,1.4);
#6306=CYLINDRICAL_SURFACE('',#6981,0.17);
#6307=CYLINDRICAL_SURFACE('',#6984,0.17);
#6308=CYLINDRICAL_SURFACE('',#6987,0.41);
#6309=CYLINDRICAL_SURFACE('',#7000,1.4);
#6310=CYLINDRICAL_SURFACE('',#7010,1.4);
#6311=CYLINDRICAL_SURFACE('',#7012,0.3);
#6312=CYLINDRICAL_SURFACE('',#7019,0.4);
#6313=CYLINDRICAL_SURFACE('',#7024,0.6);
#6314=CYLINDRICAL_SURFACE('',#7027,0.4);
#6315=CYLINDRICAL_SURFACE('',#7035,0.3);
#6316=CYLINDRICAL_SURFACE('',#7037,0.6);
#6317=CYLINDRICAL_SURFACE('',#7046,0.15);
#6318=CYLINDRICAL_SURFACE('',#7049,0.15);
#6319=CYLINDRICAL_SURFACE('',#7051,0.15);
#6320=CYLINDRICAL_SURFACE('',#7053,0.15);
#6321=CYLINDRICAL_SURFACE('',#7056,0.3);
#6322=CYLINDRICAL_SURFACE('',#7061,0.3);
#6323=CYLINDRICAL_SURFACE('',#7066,0.17);
#6324=CYLINDRICAL_SURFACE('',#7068,0.17);
#6325=CYLINDRICAL_SURFACE('',#7092,0.4);
#6326=CYLINDRICAL_SURFACE('',#7094,0.4);
#6327=CYLINDRICAL_SURFACE('',#7116,0.1);
#6328=CYLINDRICAL_SURFACE('',#7120,0.1);
#6329=CYLINDRICAL_SURFACE('',#7134,0.3);
#6330=CYLINDRICAL_SURFACE('',#7139,0.3);
#6331=CYLINDRICAL_SURFACE('',#7148,0.15);
#6332=CYLINDRICAL_SURFACE('',#7151,0.15);
#6333=CYLINDRICAL_SURFACE('',#7153,0.15);
#6334=CYLINDRICAL_SURFACE('',#7155,0.15);
#6335=CYLINDRICAL_SURFACE('',#7174,0.17);
#6336=CYLINDRICAL_SURFACE('',#7176,0.17);
#6337=CYLINDRICAL_SURFACE('',#7200,0.4);
#6338=CYLINDRICAL_SURFACE('',#7202,0.4);
#6339=CYLINDRICAL_SURFACE('',#7224,0.1);
#6340=CYLINDRICAL_SURFACE('',#7228,0.1);
#6341=CYLINDRICAL_SURFACE('',#7242,0.3);
#6342=CYLINDRICAL_SURFACE('',#7247,0.3);
#6343=CYLINDRICAL_SURFACE('',#7252,0.35);
#6344=CYLINDRICAL_SURFACE('',#7255,0.35);
#6345=CYLINDRICAL_SURFACE('',#7261,0.25);
#6346=CYLINDRICAL_SURFACE('',#7267,0.25);
#6347=CYLINDRICAL_SURFACE('',#7273,0.25);
#6348=CYLINDRICAL_SURFACE('',#7279,0.25);
#6349=CYLINDRICAL_SURFACE('',#7282,0.15);
#6350=CYLINDRICAL_SURFACE('',#7284,0.15);
#6351=CYLINDRICAL_SURFACE('',#7286,0.15);
#6352=CYLINDRICAL_SURFACE('',#7288,0.15);
#6353=CYLINDRICAL_SURFACE('',#7292,0.08);
#6354=CYLINDRICAL_SURFACE('',#7297,0.08);
#6355=CYLINDRICAL_SURFACE('',#7305,0.14635);
#6356=CYLINDRICAL_SURFACE('',#7307,0.14635);
#6357=CYLINDRICAL_SURFACE('',#7308,0.14635);
#6358=CYLINDRICAL_SURFACE('',#7309,0.14635);
#6359=CYLINDRICAL_SURFACE('',#7310,0.14635);
#6360=CYLINDRICAL_SURFACE('',#7311,0.14635);
#6361=CYLINDRICAL_SURFACE('',#7312,0.14635);
#6362=CYLINDRICAL_SURFACE('',#7313,0.14635);
#6363=CYLINDRICAL_SURFACE('',#7314,0.14635);
#6364=CYLINDRICAL_SURFACE('',#7315,0.14635);
#6365=CYLINDRICAL_SURFACE('',#7316,0.14635);
#6366=CYLINDRICAL_SURFACE('',#7317,0.14635);
#6367=CYLINDRICAL_SURFACE('',#7318,0.14635);
#6368=CYLINDRICAL_SURFACE('',#7319,0.14635);
#6369=CYLINDRICAL_SURFACE('',#7320,0.14635);
#6370=CYLINDRICAL_SURFACE('',#7321,0.14635);
#6371=CYLINDRICAL_SURFACE('',#7322,0.14635);
#6372=CYLINDRICAL_SURFACE('',#7323,0.14635);
#6373=CYLINDRICAL_SURFACE('',#7324,0.14635);
#6374=CYLINDRICAL_SURFACE('',#7325,0.14635);
#6375=CYLINDRICAL_SURFACE('',#7326,0.14635);
#6376=CYLINDRICAL_SURFACE('',#7327,0.14635);
#6377=CYLINDRICAL_SURFACE('',#7328,0.14635);
#6378=CYLINDRICAL_SURFACE('',#7329,0.14635);
#6379=CYLINDRICAL_SURFACE('',#7330,0.14635);
#6380=CYLINDRICAL_SURFACE('',#7331,0.14635);
#6381=CYLINDRICAL_SURFACE('',#7332,0.14635);
#6382=CYLINDRICAL_SURFACE('',#7333,0.14635);
#6383=CYLINDRICAL_SURFACE('',#7334,0.14635);
#6384=CYLINDRICAL_SURFACE('',#7335,0.14635);
#6385=CYLINDRICAL_SURFACE('',#7336,0.117775);
#6386=CYLINDRICAL_SURFACE('',#7338,0.117775);
#6387=CYLINDRICAL_SURFACE('',#7339,0.117775);
#6388=CYLINDRICAL_SURFACE('',#7340,0.117775);
#6389=CYLINDRICAL_SURFACE('',#7341,0.117775);
#6390=CYLINDRICAL_SURFACE('',#7342,0.117775);
#6391=CYLINDRICAL_SURFACE('',#7343,0.117775);
#6392=CYLINDRICAL_SURFACE('',#7344,0.117775);
#6393=CYLINDRICAL_SURFACE('',#7345,0.117775);
#6394=CYLINDRICAL_SURFACE('',#7346,0.117775);
#6395=CYLINDRICAL_SURFACE('',#7347,0.117775);
#6396=CYLINDRICAL_SURFACE('',#7348,0.117775);
#6397=CYLINDRICAL_SURFACE('',#7349,0.117775);
#6398=CYLINDRICAL_SURFACE('',#7350,0.117775);
#6399=CYLINDRICAL_SURFACE('',#7351,0.117775);
#6400=CYLINDRICAL_SURFACE('',#7352,0.117775);
#6401=CYLINDRICAL_SURFACE('',#7353,0.117775);
#6402=CYLINDRICAL_SURFACE('',#7354,0.117775);
#6403=CYLINDRICAL_SURFACE('',#7355,0.117775);
#6404=CYLINDRICAL_SURFACE('',#7356,0.117775);
#6405=CYLINDRICAL_SURFACE('',#7357,0.117775);
#6406=CYLINDRICAL_SURFACE('',#7358,0.117775);
#6407=CYLINDRICAL_SURFACE('',#7359,0.117775);
#6408=CYLINDRICAL_SURFACE('',#7360,0.117775);
#6409=CYLINDRICAL_SURFACE('',#7361,0.117775);
#6410=CYLINDRICAL_SURFACE('',#7362,0.117775);
#6411=CYLINDRICAL_SURFACE('',#7363,0.117775);
#6412=CYLINDRICAL_SURFACE('',#7364,0.117775);
#6413=CYLINDRICAL_SURFACE('',#7365,0.117775);
#6414=CYLINDRICAL_SURFACE('',#7366,0.117775);
#6415=CYLINDRICAL_SURFACE('',#7370,0.117775);
#6416=CYLINDRICAL_SURFACE('',#7372,0.14635);
#6417=CYLINDRICAL_SURFACE('',#7382,0.275);
#6418=CYLINDRICAL_SURFACE('',#7387,0.12645);
#6419=CYLINDRICAL_SURFACE('',#7389,0.12645);
#6420=CYLINDRICAL_SURFACE('',#7391,0.12645);
#6421=CYLINDRICAL_SURFACE('',#7392,0.12645);
#6422=CYLINDRICAL_SURFACE('',#7393,0.12645);
#6423=CYLINDRICAL_SURFACE('',#7395,0.1543);
#6424=CYLINDRICAL_SURFACE('',#7397,0.1543);
#6425=CYLINDRICAL_SURFACE('',#7398,0.1543);
#6426=CYLINDRICAL_SURFACE('',#7399,0.1543);
#6427=CYLINDRICAL_SURFACE('',#7400,0.1543);
#6428=CYLINDRICAL_SURFACE('',#7402,0.1543);
#6429=CYLINDRICAL_SURFACE('',#7404,0.12645);
#6430=CYLINDRICAL_SURFACE('',#7421,0.41);
#6431=CYLINDRICAL_SURFACE('',#7424,0.6);
#6432=ADVANCED_FACE('',(#813),#6301,.F.);
#6433=ADVANCED_FACE('',(#814),#6302,.F.);
#6434=ADVANCED_FACE('',(#815),#6303,.F.);
#6435=ADVANCED_FACE('',(#816),#653,.F.);
#6436=ADVANCED_FACE('',(#817),#654,.F.);
#6437=ADVANCED_FACE('',(#818),#655,.T.);
#6438=ADVANCED_FACE('',(#819),#656,.T.);
#6439=ADVANCED_FACE('',(#820),#657,.F.);
#6440=ADVANCED_FACE('',(#821),#658,.F.);
#6441=ADVANCED_FACE('',(#822),#659,.T.);
#6442=ADVANCED_FACE('',(#823,#586,#587,#588),#660,.T.);
#6443=ADVANCED_FACE('',(#824),#661,.T.);
#6444=ADVANCED_FACE('',(#825),#662,.F.);
#6445=ADVANCED_FACE('',(#826),#663,.T.);
#6446=ADVANCED_FACE('',(#827),#664,.T.);
#6447=ADVANCED_FACE('',(#828),#665,.T.);
#6448=ADVANCED_FACE('',(#829),#666,.T.);
#6449=ADVANCED_FACE('',(#830),#667,.T.);
#6450=ADVANCED_FACE('',(#831,#589,#590,#591),#668,.F.);
#6451=ADVANCED_FACE('',(#832),#6304,.T.);
#6452=ADVANCED_FACE('',(#833),#669,.T.);
#6453=ADVANCED_FACE('',(#834),#670,.T.);
#6454=ADVANCED_FACE('',(#835),#671,.T.);
#6455=ADVANCED_FACE('',(#836),#672,.T.);
#6456=ADVANCED_FACE('',(#837),#673,.T.);
#6457=ADVANCED_FACE('',(#838),#674,.T.);
#6458=ADVANCED_FACE('',(#839),#6305,.T.);
#6459=ADVANCED_FACE('',(#840),#6306,.F.);
#6460=ADVANCED_FACE('',(#841),#6307,.F.);
#6461=ADVANCED_FACE('',(#842),#6308,.F.);
#6462=ADVANCED_FACE('',(#843),#675,.T.);
#6463=ADVANCED_FACE('',(#844),#676,.F.);
#6464=ADVANCED_FACE('',(#845),#677,.T.);
#6465=ADVANCED_FACE('',(#846),#678,.T.);
#6466=ADVANCED_FACE('',(#847),#679,.T.);
#6467=ADVANCED_FACE('',(#848),#680,.T.);
#6468=ADVANCED_FACE('',(#849),#681,.T.);
#6469=ADVANCED_FACE('',(#850,#592,#593,#594),#682,.F.);
#6470=ADVANCED_FACE('',(#851),#6309,.T.);
#6471=ADVANCED_FACE('',(#852),#683,.T.);
#6472=ADVANCED_FACE('',(#853),#684,.T.);
#6473=ADVANCED_FACE('',(#854),#685,.T.);
#6474=ADVANCED_FACE('',(#855),#686,.T.);
#6475=ADVANCED_FACE('',(#856),#687,.T.);
#6476=ADVANCED_FACE('',(#857),#688,.T.);
#6477=ADVANCED_FACE('',(#858,#595,#596,#597),#689,.T.);
#6478=ADVANCED_FACE('',(#859),#6310,.T.);
#6479=ADVANCED_FACE('',(#860),#6311,.T.);
#6480=ADVANCED_FACE('',(#861,#598),#690,.F.);
#6481=ADVANCED_FACE('',(#862,#599),#691,.F.);
#6482=ADVANCED_FACE('',(#863),#6312,.T.);
#6483=ADVANCED_FACE('',(#864,#600),#692,.T.);
#6484=ADVANCED_FACE('',(#865),#6313,.T.);
#6485=ADVANCED_FACE('',(#866),#693,.F.);
#6486=ADVANCED_FACE('',(#867),#6314,.T.);
#6487=ADVANCED_FACE('',(#868),#694,.T.);
#6488=ADVANCED_FACE('',(#869),#695,.F.);
#6489=ADVANCED_FACE('',(#870),#696,.F.);
#6490=ADVANCED_FACE('',(#871),#697,.F.);
#6491=ADVANCED_FACE('',(#872),#6315,.F.);
#6492=ADVANCED_FACE('',(#873),#6316,.T.);
#6493=ADVANCED_FACE('',(#874),#698,.T.);
#6494=ADVANCED_FACE('',(#875,#601,#602,#603),#699,.F.);
#6495=ADVANCED_FACE('',(#876),#6317,.F.);
#6496=ADVANCED_FACE('',(#877),#6318,.F.);
#6497=ADVANCED_FACE('',(#878),#6319,.F.);
#6498=ADVANCED_FACE('',(#879),#6320,.F.);
#6499=ADVANCED_FACE('',(#880),#6321,.F.);
#6500=ADVANCED_FACE('',(#881,#604),#700,.F.);
#6501=ADVANCED_FACE('',(#882),#6322,.F.);
#6502=ADVANCED_FACE('',(#883,#605),#701,.F.);
#6503=ADVANCED_FACE('',(#884),#6323,.F.);
#6504=ADVANCED_FACE('',(#885),#6324,.F.);
#6505=ADVANCED_FACE('',(#886),#702,.F.);
#6506=ADVANCED_FACE('',(#887),#703,.F.);
#6507=ADVANCED_FACE('',(#888),#704,.F.);
#6508=ADVANCED_FACE('',(#889),#705,.F.);
#6509=ADVANCED_FACE('',(#890),#706,.F.);
#6510=ADVANCED_FACE('',(#891),#707,.F.);
#6511=ADVANCED_FACE('',(#892),#708,.F.);
#6512=ADVANCED_FACE('',(#893,#606),#709,.F.);
#6513=ADVANCED_FACE('',(#894,#607),#710,.F.);
#6514=ADVANCED_FACE('',(#895),#711,.F.);
#6515=ADVANCED_FACE('',(#896),#712,.F.);
#6516=ADVANCED_FACE('',(#897),#713,.F.);
#6517=ADVANCED_FACE('',(#898),#714,.F.);
#6518=ADVANCED_FACE('',(#899),#715,.F.);
#6519=ADVANCED_FACE('',(#900),#716,.T.);
#6520=ADVANCED_FACE('',(#901),#717,.T.);
#6521=ADVANCED_FACE('',(#902),#718,.T.);
#6522=ADVANCED_FACE('',(#903),#719,.T.);
#6523=ADVANCED_FACE('',(#904),#720,.T.);
#6524=ADVANCED_FACE('',(#905,#608),#721,.F.);
#6525=ADVANCED_FACE('',(#906),#6325,.T.);
#6526=ADVANCED_FACE('',(#907),#6326,.T.);
#6527=ADVANCED_FACE('',(#908),#722,.T.);
#6528=ADVANCED_FACE('',(#909),#92,.T.);
#6529=ADVANCED_FACE('',(#910),#93,.T.);
#6530=ADVANCED_FACE('',(#911),#94,.T.);
#6531=ADVANCED_FACE('',(#912),#95,.T.);
#6532=ADVANCED_FACE('',(#913,#609,#610,#611),#723,.F.);
#6533=ADVANCED_FACE('',(#914),#724,.F.);
#6534=ADVANCED_FACE('',(#915),#96,.T.);
#6535=ADVANCED_FACE('',(#916),#97,.T.);
#6536=ADVANCED_FACE('',(#917),#98,.T.);
#6537=ADVANCED_FACE('',(#918),#725,.T.);
#6538=ADVANCED_FACE('',(#919),#99,.T.);
#6539=ADVANCED_FACE('',(#920),#100,.T.);
#6540=ADVANCED_FACE('',(#921),#726,.F.);
#6541=ADVANCED_FACE('',(#922),#101,.T.);
#6542=ADVANCED_FACE('',(#923),#102,.T.);
#6543=ADVANCED_FACE('',(#924),#727,.T.);
#6544=ADVANCED_FACE('',(#925),#103,.T.);
#6545=ADVANCED_FACE('',(#926),#104,.T.);
#6546=ADVANCED_FACE('',(#927),#105,.T.);
#6547=ADVANCED_FACE('',(#928),#106,.T.);
#6548=ADVANCED_FACE('',(#929),#728,.T.);
#6549=ADVANCED_FACE('',(#930),#107,.T.);
#6550=ADVANCED_FACE('',(#931),#108,.T.);
#6551=ADVANCED_FACE('',(#932),#729,.F.);
#6552=ADVANCED_FACE('',(#933),#109,.T.);
#6553=ADVANCED_FACE('',(#934),#110,.T.);
#6554=ADVANCED_FACE('',(#935),#76,.F.);
#6555=ADVANCED_FACE('',(#936),#77,.F.);
#6556=ADVANCED_FACE('',(#937),#78,.F.);
#6557=ADVANCED_FACE('',(#938),#6327,.F.);
#6558=ADVANCED_FACE('',(#939),#111,.T.);
#6559=ADVANCED_FACE('',(#940),#79,.F.);
#6560=ADVANCED_FACE('',(#941),#6328,.F.);
#6561=ADVANCED_FACE('',(#942),#112,.T.);
#6562=ADVANCED_FACE('',(#943),#113,.T.);
#6563=ADVANCED_FACE('',(#944),#114,.T.);
#6564=ADVANCED_FACE('',(#945),#115,.T.);
#6565=ADVANCED_FACE('',(#946),#730,.T.);
#6566=ADVANCED_FACE('',(#947),#80,.T.);
#6567=ADVANCED_FACE('',(#948),#81,.T.);
#6568=ADVANCED_FACE('',(#949),#82,.T.);
#6569=ADVANCED_FACE('',(#950),#6329,.T.);
#6570=ADVANCED_FACE('',(#951),#116,.F.);
#6571=ADVANCED_FACE('',(#952),#83,.T.);
#6572=ADVANCED_FACE('',(#953),#6330,.T.);
#6573=ADVANCED_FACE('',(#954),#117,.F.);
#6574=ADVANCED_FACE('',(#955),#118,.F.);
#6575=ADVANCED_FACE('',(#956),#119,.F.);
#6576=ADVANCED_FACE('',(#957),#120,.F.);
#6577=ADVANCED_FACE('',(#958),#121,.F.);
#6578=ADVANCED_FACE('',(#959),#122,.F.);
#6579=ADVANCED_FACE('',(#960),#731,.F.);
#6580=ADVANCED_FACE('',(#961,#612,#613,#614,#615,#616,#617),#732,.T.);
#6581=ADVANCED_FACE('',(#962),#123,.F.);
#6582=ADVANCED_FACE('',(#963),#733,.F.);
#6583=ADVANCED_FACE('',(#964,#618,#619,#620),#734,.F.);
#6584=ADVANCED_FACE('',(#965),#6331,.F.);
#6585=ADVANCED_FACE('',(#966),#6332,.F.);
#6586=ADVANCED_FACE('',(#967),#6333,.F.);
#6587=ADVANCED_FACE('',(#968),#6334,.F.);
#6588=ADVANCED_FACE('',(#969),#735,.F.);
#6589=ADVANCED_FACE('',(#970),#736,.F.);
#6590=ADVANCED_FACE('',(#971),#737,.F.);
#6591=ADVANCED_FACE('',(#972),#738,.F.);
#6592=ADVANCED_FACE('',(#973),#739,.F.);
#6593=ADVANCED_FACE('',(#974),#740,.F.);
#6594=ADVANCED_FACE('',(#975,#621),#741,.F.);
#6595=ADVANCED_FACE('',(#976),#742,.F.);
#6596=ADVANCED_FACE('',(#977),#743,.F.);
#6597=ADVANCED_FACE('',(#978),#744,.F.);
#6598=ADVANCED_FACE('',(#979),#745,.F.);
#6599=ADVANCED_FACE('',(#980),#746,.F.);
#6600=ADVANCED_FACE('',(#981),#747,.F.);
#6601=ADVANCED_FACE('',(#982,#622),#748,.F.);
#6602=ADVANCED_FACE('',(#983),#6335,.F.);
#6603=ADVANCED_FACE('',(#984),#6336,.F.);
#6604=ADVANCED_FACE('',(#985),#749,.F.);
#6605=ADVANCED_FACE('',(#986),#750,.F.);
#6606=ADVANCED_FACE('',(#987),#751,.F.);
#6607=ADVANCED_FACE('',(#988),#752,.F.);
#6608=ADVANCED_FACE('',(#989),#753,.F.);
#6609=ADVANCED_FACE('',(#990),#754,.F.);
#6610=ADVANCED_FACE('',(#991),#755,.F.);
#6611=ADVANCED_FACE('',(#992,#623),#756,.F.);
#6612=ADVANCED_FACE('',(#993,#624),#757,.F.);
#6613=ADVANCED_FACE('',(#994),#758,.F.);
#6614=ADVANCED_FACE('',(#995),#759,.F.);
#6615=ADVANCED_FACE('',(#996),#760,.F.);
#6616=ADVANCED_FACE('',(#997),#761,.F.);
#6617=ADVANCED_FACE('',(#998),#762,.F.);
#6618=ADVANCED_FACE('',(#999),#763,.T.);
#6619=ADVANCED_FACE('',(#1000),#764,.T.);
#6620=ADVANCED_FACE('',(#1001),#765,.T.);
#6621=ADVANCED_FACE('',(#1002),#766,.T.);
#6622=ADVANCED_FACE('',(#1003),#767,.T.);
#6623=ADVANCED_FACE('',(#1004,#625),#768,.F.);
#6624=ADVANCED_FACE('',(#1005),#6337,.T.);
#6625=ADVANCED_FACE('',(#1006),#6338,.T.);
#6626=ADVANCED_FACE('',(#1007),#769,.T.);
#6627=ADVANCED_FACE('',(#1008),#124,.T.);
#6628=ADVANCED_FACE('',(#1009),#125,.T.);
#6629=ADVANCED_FACE('',(#1010),#126,.T.);
#6630=ADVANCED_FACE('',(#1011),#127,.T.);
#6631=ADVANCED_FACE('',(#1012,#626,#627,#628),#770,.F.);
#6632=ADVANCED_FACE('',(#1013),#771,.F.);
#6633=ADVANCED_FACE('',(#1014),#128,.T.);
#6634=ADVANCED_FACE('',(#1015),#129,.T.);
#6635=ADVANCED_FACE('',(#1016),#130,.T.);
#6636=ADVANCED_FACE('',(#1017),#772,.T.);
#6637=ADVANCED_FACE('',(#1018),#131,.T.);
#6638=ADVANCED_FACE('',(#1019),#132,.T.);
#6639=ADVANCED_FACE('',(#1020),#773,.F.);
#6640=ADVANCED_FACE('',(#1021),#133,.T.);
#6641=ADVANCED_FACE('',(#1022),#134,.T.);
#6642=ADVANCED_FACE('',(#1023),#774,.T.);
#6643=ADVANCED_FACE('',(#1024),#135,.T.);
#6644=ADVANCED_FACE('',(#1025),#136,.T.);
#6645=ADVANCED_FACE('',(#1026),#137,.T.);
#6646=ADVANCED_FACE('',(#1027),#138,.T.);
#6647=ADVANCED_FACE('',(#1028),#775,.T.);
#6648=ADVANCED_FACE('',(#1029),#139,.T.);
#6649=ADVANCED_FACE('',(#1030),#140,.T.);
#6650=ADVANCED_FACE('',(#1031),#776,.F.);
#6651=ADVANCED_FACE('',(#1032),#141,.T.);
#6652=ADVANCED_FACE('',(#1033),#142,.T.);
#6653=ADVANCED_FACE('',(#1034),#84,.F.);
#6654=ADVANCED_FACE('',(#1035),#85,.F.);
#6655=ADVANCED_FACE('',(#1036),#86,.F.);
#6656=ADVANCED_FACE('',(#1037),#6339,.F.);
#6657=ADVANCED_FACE('',(#1038),#143,.T.);
#6658=ADVANCED_FACE('',(#1039),#87,.F.);
#6659=ADVANCED_FACE('',(#1040),#6340,.F.);
#6660=ADVANCED_FACE('',(#1041),#144,.T.);
#6661=ADVANCED_FACE('',(#1042),#145,.T.);
#6662=ADVANCED_FACE('',(#1043),#146,.T.);
#6663=ADVANCED_FACE('',(#1044),#147,.T.);
#6664=ADVANCED_FACE('',(#1045),#777,.T.);
#6665=ADVANCED_FACE('',(#1046),#88,.T.);
#6666=ADVANCED_FACE('',(#1047),#89,.T.);
#6667=ADVANCED_FACE('',(#1048),#90,.T.);
#6668=ADVANCED_FACE('',(#1049),#6341,.T.);
#6669=ADVANCED_FACE('',(#1050),#148,.F.);
#6670=ADVANCED_FACE('',(#1051),#91,.T.);
#6671=ADVANCED_FACE('',(#1052),#6342,.T.);
#6672=ADVANCED_FACE('',(#1053),#149,.F.);
#6673=ADVANCED_FACE('',(#1054),#150,.F.);
#6674=ADVANCED_FACE('',(#1055),#151,.F.);
#6675=ADVANCED_FACE('',(#1056),#152,.F.);
#6676=ADVANCED_FACE('',(#1057),#153,.F.);
#6677=ADVANCED_FACE('',(#1058),#154,.F.);
#6678=ADVANCED_FACE('',(#1059),#778,.F.);
#6679=ADVANCED_FACE('',(#1060,#629,#630,#631,#632,#633,#634),#779,.T.);
#6680=ADVANCED_FACE('',(#1061),#155,.F.);
#6681=ADVANCED_FACE('',(#1062),#780,.F.);
#6682=ADVANCED_FACE('',(#1063),#6343,.F.);
#6683=ADVANCED_FACE('',(#1064),#6344,.F.);
#6684=ADVANCED_FACE('',(#1065,#635),#781,.T.);
#6685=ADVANCED_FACE('',(#1066),#6345,.T.);
#6686=ADVANCED_FACE('',(#1067),#782,.F.);
#6687=ADVANCED_FACE('',(#1068,#636),#783,.T.);
#6688=ADVANCED_FACE('',(#1069),#6346,.T.);
#6689=ADVANCED_FACE('',(#1070),#784,.F.);
#6690=ADVANCED_FACE('',(#1071,#637),#785,.T.);
#6691=ADVANCED_FACE('',(#1072),#6347,.T.);
#6692=ADVANCED_FACE('',(#1073),#786,.F.);
#6693=ADVANCED_FACE('',(#1074,#638),#787,.T.);
#6694=ADVANCED_FACE('',(#1075),#6348,.T.);
#6695=ADVANCED_FACE('',(#1076),#788,.F.);
#6696=ADVANCED_FACE('',(#1077),#6349,.T.);
#6697=ADVANCED_FACE('',(#1078),#6350,.T.);
#6698=ADVANCED_FACE('',(#1079),#6351,.T.);
#6699=ADVANCED_FACE('',(#1080),#6352,.T.);
#6700=ADVANCED_FACE('',(#1081),#156,.F.);
#6701=ADVANCED_FACE('',(#1082),#6353,.T.);
#6702=ADVANCED_FACE('',(#1083),#157,.F.);
#6703=ADVANCED_FACE('',(#1084),#158,.F.);
#6704=ADVANCED_FACE('',(#1085),#159,.F.);
#6705=ADVANCED_FACE('',(#1086),#6354,.T.);
#6706=ADVANCED_FACE('',(#1087),#160,.F.);
#6707=ADVANCED_FACE('',(#1088),#161,.F.);
#6708=ADVANCED_FACE('',(#1089),#789,.F.);
#6709=ADVANCED_FACE('',(#1090),#162,.F.);
#6710=ADVANCED_FACE('',(#1091),#163,.F.);
#6711=ADVANCED_FACE('',(#1092),#164,.F.);
#6712=ADVANCED_FACE('',(#1093,#639,#640),#790,.T.);
#6713=ADVANCED_FACE('',(#1094),#791,.F.);
#6714=ADVANCED_FACE('',(#1095),#165,.F.);
#6715=ADVANCED_FACE('',(#1096),#166,.F.);
#6716=ADVANCED_FACE('',(#1097,#641,#642,#643,#644,#645,#646),#792,.F.);
#6717=ADVANCED_FACE('',(#1098),#167,.F.);
#6718=ADVANCED_FACE('',(#1099),#6355,.T.);
#6719=ADVANCED_FACE('',(#1100),#6356,.T.);
#6720=ADVANCED_FACE('',(#1101),#6357,.T.);
#6721=ADVANCED_FACE('',(#1102),#6358,.T.);
#6722=ADVANCED_FACE('',(#1103),#6359,.T.);
#6723=ADVANCED_FACE('',(#1104),#6360,.T.);
#6724=ADVANCED_FACE('',(#1105),#6361,.T.);
#6725=ADVANCED_FACE('',(#1106),#6362,.T.);
#6726=ADVANCED_FACE('',(#1107),#6363,.T.);
#6727=ADVANCED_FACE('',(#1108),#6364,.T.);
#6728=ADVANCED_FACE('',(#1109),#6365,.T.);
#6729=ADVANCED_FACE('',(#1110),#6366,.T.);
#6730=ADVANCED_FACE('',(#1111),#6367,.T.);
#6731=ADVANCED_FACE('',(#1112),#6368,.T.);
#6732=ADVANCED_FACE('',(#1113),#6369,.T.);
#6733=ADVANCED_FACE('',(#1114),#6370,.T.);
#6734=ADVANCED_FACE('',(#1115),#6371,.T.);
#6735=ADVANCED_FACE('',(#1116),#6372,.T.);
#6736=ADVANCED_FACE('',(#1117),#6373,.T.);
#6737=ADVANCED_FACE('',(#1118),#6374,.T.);
#6738=ADVANCED_FACE('',(#1119),#6375,.T.);
#6739=ADVANCED_FACE('',(#1120),#6376,.T.);
#6740=ADVANCED_FACE('',(#1121),#6377,.T.);
#6741=ADVANCED_FACE('',(#1122),#6378,.T.);
#6742=ADVANCED_FACE('',(#1123),#6379,.T.);
#6743=ADVANCED_FACE('',(#1124),#6380,.T.);
#6744=ADVANCED_FACE('',(#1125),#6381,.T.);
#6745=ADVANCED_FACE('',(#1126),#6382,.T.);
#6746=ADVANCED_FACE('',(#1127),#6383,.T.);
#6747=ADVANCED_FACE('',(#1128),#6384,.T.);
#6748=ADVANCED_FACE('',(#1129),#6385,.T.);
#6749=ADVANCED_FACE('',(#1130),#6386,.T.);
#6750=ADVANCED_FACE('',(#1131),#6387,.T.);
#6751=ADVANCED_FACE('',(#1132),#6388,.T.);
#6752=ADVANCED_FACE('',(#1133),#6389,.T.);
#6753=ADVANCED_FACE('',(#1134),#6390,.T.);
#6754=ADVANCED_FACE('',(#1135),#6391,.T.);
#6755=ADVANCED_FACE('',(#1136),#6392,.T.);
#6756=ADVANCED_FACE('',(#1137),#6393,.T.);
#6757=ADVANCED_FACE('',(#1138),#6394,.T.);
#6758=ADVANCED_FACE('',(#1139),#6395,.T.);
#6759=ADVANCED_FACE('',(#1140),#6396,.T.);
#6760=ADVANCED_FACE('',(#1141),#6397,.T.);
#6761=ADVANCED_FACE('',(#1142),#6398,.T.);
#6762=ADVANCED_FACE('',(#1143),#6399,.T.);
#6763=ADVANCED_FACE('',(#1144),#6400,.T.);
#6764=ADVANCED_FACE('',(#1145),#6401,.T.);
#6765=ADVANCED_FACE('',(#1146),#6402,.T.);
#6766=ADVANCED_FACE('',(#1147),#6403,.T.);
#6767=ADVANCED_FACE('',(#1148),#6404,.T.);
#6768=ADVANCED_FACE('',(#1149),#6405,.T.);
#6769=ADVANCED_FACE('',(#1150),#6406,.T.);
#6770=ADVANCED_FACE('',(#1151),#6407,.T.);
#6771=ADVANCED_FACE('',(#1152),#6408,.T.);
#6772=ADVANCED_FACE('',(#1153),#6409,.T.);
#6773=ADVANCED_FACE('',(#1154),#6410,.T.);
#6774=ADVANCED_FACE('',(#1155),#6411,.T.);
#6775=ADVANCED_FACE('',(#1156),#6412,.T.);
#6776=ADVANCED_FACE('',(#1157),#6413,.T.);
#6777=ADVANCED_FACE('',(#1158),#6414,.T.);
#6778=ADVANCED_FACE('',(#1159),#75,.T.);
#6779=ADVANCED_FACE('',(#1160),#168,.F.);
#6780=ADVANCED_FACE('',(#1161),#6415,.T.);
#6781=ADVANCED_FACE('',(#1162),#169,.F.);
#6782=ADVANCED_FACE('',(#1163),#6416,.T.);
#6783=ADVANCED_FACE('',(#1164),#793,.F.);
#6784=ADVANCED_FACE('',(#1165),#794,.F.);
#6785=ADVANCED_FACE('',(#1166),#795,.F.);
#6786=ADVANCED_FACE('',(#1167),#796,.F.);
#6787=ADVANCED_FACE('',(#1168),#797,.F.);
#6788=ADVANCED_FACE('',(#1169),#798,.F.);
#6789=ADVANCED_FACE('',(#1170),#799,.F.);
#6790=ADVANCED_FACE('',(#1171,#647),#800,.T.);
#6791=ADVANCED_FACE('',(#1172),#6417,.T.);
#6792=ADVANCED_FACE('',(#1173,#648),#801,.F.);
#6793=ADVANCED_FACE('',(#1174),#802,.T.);
#6794=ADVANCED_FACE('',(#1175),#6418,.F.);
#6795=ADVANCED_FACE('',(#1176),#6419,.F.);
#6796=ADVANCED_FACE('',(#1177),#6420,.F.);
#6797=ADVANCED_FACE('',(#1178),#6421,.F.);
#6798=ADVANCED_FACE('',(#1179),#6422,.F.);
#6799=ADVANCED_FACE('',(#1180),#6423,.F.);
#6800=ADVANCED_FACE('',(#1181),#6424,.F.);
#6801=ADVANCED_FACE('',(#1182),#6425,.F.);
#6802=ADVANCED_FACE('',(#1183),#6426,.F.);
#6803=ADVANCED_FACE('',(#1184),#6427,.F.);
#6804=ADVANCED_FACE('',(#1185),#6428,.F.);
#6805=ADVANCED_FACE('',(#1186),#170,.F.);
#6806=ADVANCED_FACE('',(#1187),#171,.F.);
#6807=ADVANCED_FACE('',(#1188,#649),#803,.T.);
#6808=ADVANCED_FACE('',(#1189),#6429,.F.);
#6809=ADVANCED_FACE('',(#1190),#804,.T.);
#6810=ADVANCED_FACE('',(#1191),#805,.T.);
#6811=ADVANCED_FACE('',(#1192),#806,.T.);
#6812=ADVANCED_FACE('',(#1193),#807,.T.);
#6813=ADVANCED_FACE('',(#1194),#808,.T.);
#6814=ADVANCED_FACE('',(#1195),#809,.T.);
#6815=ADVANCED_FACE('',(#1196,#650),#810,.F.);
#6816=ADVANCED_FACE('',(#1197),#6430,.F.);
#6817=ADVANCED_FACE('',(#1198),#6431,.T.);
#6818=ADVANCED_FACE('',(#1199,#651),#811,.T.);
#6819=ADVANCED_FACE('',(#1200,#652),#812,.F.);
#6820=CLOSED_SHELL('',(#6432,#6433,#6434,#6435,#6436,#6437,#6438,#6439,
#6440,#6441,#6442,#6443,#6444,#6445,#6446,#6447,#6448,#6449,#6450,#6451,
#6452,#6453,#6454,#6455,#6456,#6457,#6458));
#6821=CLOSED_SHELL('',(#6459,#6460,#6461,#6462,#6463,#6464,#6465,#6466,
#6467,#6468,#6469,#6470,#6471,#6472,#6473,#6474,#6475,#6476,#6477,#6478));
#6822=CLOSED_SHELL('',(#6479,#6480,#6481,#6482,#6483,#6484,#6485,#6486,
#6487));
#6823=CLOSED_SHELL('',(#6488,#6489,#6490,#6491,#6492,#6493));
#6824=CLOSED_SHELL('',(#6494,#6495,#6496,#6497,#6498,#6499,#6500,#6501,
#6502,#6503,#6504,#6505,#6506,#6507,#6508,#6509,#6510,#6511,#6512,#6513,
#6514,#6515,#6516,#6517,#6518,#6519,#6520,#6521,#6522,#6523,#6524,#6525,
#6526,#6527,#6528,#6529,#6530,#6531,#6532,#6533,#6534,#6535,#6536,#6537,
#6538,#6539,#6540,#6541,#6542,#6543,#6544,#6545,#6546,#6547,#6548,#6549,
#6550,#6551,#6552,#6553,#6554,#6555,#6556,#6557,#6558,#6559,#6560,#6561,
#6562,#6563,#6564,#6565,#6566,#6567,#6568,#6569,#6570,#6571,#6572,#6573,
#6574,#6575,#6576,#6577,#6578,#6579,#6580,#6581,#6582));
#6825=CLOSED_SHELL('',(#6583,#6584,#6585,#6586,#6587,#6588,#6589,#6590,
#6591,#6592,#6593,#6594,#6595,#6596,#6597,#6598,#6599,#6600,#6601,#6602,
#6603,#6604,#6605,#6606,#6607,#6608,#6609,#6610,#6611,#6612,#6613,#6614,
#6615,#6616,#6617,#6618,#6619,#6620,#6621,#6622,#6623,#6624,#6625,#6626,
#6627,#6628,#6629,#6630,#6631,#6632,#6633,#6634,#6635,#6636,#6637,#6638,
#6639,#6640,#6641,#6642,#6643,#6644,#6645,#6646,#6647,#6648,#6649,#6650,
#6651,#6652,#6653,#6654,#6655,#6656,#6657,#6658,#6659,#6660,#6661,#6662,
#6663,#6664,#6665,#6666,#6667,#6668,#6669,#6670,#6671,#6672,#6673,#6674,
#6675,#6676,#6677,#6678,#6679,#6680,#6681));
#6826=CLOSED_SHELL('',(#6682,#6683,#6684,#6685,#6686,#6687,#6688,#6689,
#6690,#6691,#6692,#6693,#6694,#6695,#6696,#6697,#6698,#6699,#6700,#6701,
#6702,#6703,#6704,#6705,#6706,#6707,#6708,#6709,#6710,#6711,#6712,#6713,
#6714,#6715,#6716,#6717));
#6827=CLOSED_SHELL('',(#6718,#6719,#6720,#6721,#6722,#6723,#6724,#6725,
#6726,#6727,#6728,#6729,#6730,#6731,#6732,#6733,#6734,#6735,#6736,#6737,
#6738,#6739,#6740,#6741,#6742,#6743,#6744,#6745,#6746,#6747,#6748,#6749,
#6750,#6751,#6752,#6753,#6754,#6755,#6756,#6757,#6758,#6759,#6760,#6761,
#6762,#6763,#6764,#6765,#6766,#6767,#6768,#6769,#6770,#6771,#6772,#6773,
#6774,#6775,#6776,#6777,#6778,#6779,#6780,#6781,#6782,#6783,#6784,#6785,
#6786,#6787,#6788,#6789,#6790,#6791,#6792,#6793));
#6828=CLOSED_SHELL('',(#6794,#6795,#6796,#6797,#6798,#6799,#6800,#6801,
#6802,#6803,#6804,#6805,#6806,#6807,#6808,#6809,#6810,#6811,#6812,#6813,
#6814,#6815));
#6829=CLOSED_SHELL('',(#6816,#6817,#6818,#6819));
#6830=DERIVED_UNIT_ELEMENT(#6850,1.);
#6831=DERIVED_UNIT_ELEMENT(#19092,-3.);
#6832=DERIVED_UNIT_ELEMENT(#6850,1.);
#6833=DERIVED_UNIT_ELEMENT(#19092,-3.);
#6834=DERIVED_UNIT_ELEMENT(#6850,1.);
#6835=DERIVED_UNIT_ELEMENT(#19092,-3.);
#6836=DERIVED_UNIT_ELEMENT(#6850,1.);
#6837=DERIVED_UNIT_ELEMENT(#19092,-3.);
#6838=DERIVED_UNIT_ELEMENT(#6850,1.);
#6839=DERIVED_UNIT_ELEMENT(#19092,-3.);
#6840=DERIVED_UNIT_ELEMENT(#6850,1.);
#6841=DERIVED_UNIT_ELEMENT(#19092,-3.);
#6842=DERIVED_UNIT_ELEMENT(#6850,1.);
#6843=DERIVED_UNIT_ELEMENT(#19092,-3.);
#6844=DERIVED_UNIT_ELEMENT(#6850,1.);
#6845=DERIVED_UNIT_ELEMENT(#19092,-3.);
#6846=DERIVED_UNIT_ELEMENT(#6850,1.);
#6847=DERIVED_UNIT_ELEMENT(#19092,-3.);
#6848=DERIVED_UNIT_ELEMENT(#6850,1.);
#6849=DERIVED_UNIT_ELEMENT(#19092,-3.);
#6850=(
MASS_UNIT()
NAMED_UNIT(*)
SI_UNIT(.KILO.,.GRAM.)
);
#6851=DERIVED_UNIT((#6830,#6831));
#6852=DERIVED_UNIT((#6832,#6833));
#6853=DERIVED_UNIT((#6834,#6835));
#6854=DERIVED_UNIT((#6836,#6837));
#6855=DERIVED_UNIT((#6838,#6839));
#6856=DERIVED_UNIT((#6840,#6841));
#6857=DERIVED_UNIT((#6842,#6843));
#6858=DERIVED_UNIT((#6844,#6845));
#6859=DERIVED_UNIT((#6846,#6847));
#6860=DERIVED_UNIT((#6848,#6849));
#6861=MEASURE_REPRESENTATION_ITEM('density measure',
POSITIVE_RATIO_MEASURE(7850.),#6851);
#6862=MEASURE_REPRESENTATION_ITEM('density measure',
POSITIVE_RATIO_MEASURE(7850.),#6852);
#6863=MEASURE_REPRESENTATION_ITEM('density measure',
POSITIVE_RATIO_MEASURE(7850.),#6853);
#6864=MEASURE_REPRESENTATION_ITEM('density measure',
POSITIVE_RATIO_MEASURE(7850.),#6854);
#6865=MEASURE_REPRESENTATION_ITEM('density measure',
POSITIVE_RATIO_MEASURE(7850.),#6855);
#6866=MEASURE_REPRESENTATION_ITEM('density measure',
POSITIVE_RATIO_MEASURE(7850.),#6856);
#6867=MEASURE_REPRESENTATION_ITEM('density measure',
POSITIVE_RATIO_MEASURE(7850.),#6857);
#6868=MEASURE_REPRESENTATION_ITEM('density measure',
POSITIVE_RATIO_MEASURE(7850.),#6858);
#6869=MEASURE_REPRESENTATION_ITEM('density measure',
POSITIVE_RATIO_MEASURE(7850.),#6859);
#6870=MEASURE_REPRESENTATION_ITEM('density measure',
POSITIVE_RATIO_MEASURE(7850.),#6860);
#6871=PROPERTY_DEFINITION_REPRESENTATION(#6921,#6891);
#6872=PROPERTY_DEFINITION_REPRESENTATION(#6922,#6892);
#6873=PROPERTY_DEFINITION_REPRESENTATION(#6923,#6893);
#6874=PROPERTY_DEFINITION_REPRESENTATION(#6924,#6894);
#6875=PROPERTY_DEFINITION_REPRESENTATION(#6925,#6895);
#6876=PROPERTY_DEFINITION_REPRESENTATION(#6926,#6896);
#6877=PROPERTY_DEFINITION_REPRESENTATION(#6927,#6897);
#6878=PROPERTY_DEFINITION_REPRESENTATION(#6928,#6898);
#6879=PROPERTY_DEFINITION_REPRESENTATION(#6929,#6899);
#6880=PROPERTY_DEFINITION_REPRESENTATION(#6930,#6900);
#6881=PROPERTY_DEFINITION_REPRESENTATION(#6931,#6901);
#6882=PROPERTY_DEFINITION_REPRESENTATION(#6932,#6902);
#6883=PROPERTY_DEFINITION_REPRESENTATION(#6933,#6903);
#6884=PROPERTY_DEFINITION_REPRESENTATION(#6934,#6904);
#6885=PROPERTY_DEFINITION_REPRESENTATION(#6935,#6905);
#6886=PROPERTY_DEFINITION_REPRESENTATION(#6936,#6906);
#6887=PROPERTY_DEFINITION_REPRESENTATION(#6937,#6907);
#6888=PROPERTY_DEFINITION_REPRESENTATION(#6938,#6908);
#6889=PROPERTY_DEFINITION_REPRESENTATION(#6939,#6909);
#6890=PROPERTY_DEFINITION_REPRESENTATION(#6940,#6910);
#6891=REPRESENTATION('material name',(#6911),#19079);
#6892=REPRESENTATION('density',(#6861),#19079);
#6893=REPRESENTATION('material name',(#6912),#19080);
#6894=REPRESENTATION('density',(#6862),#19080);
#6895=REPRESENTATION('material name',(#6913),#19081);
#6896=REPRESENTATION('density',(#6863),#19081);
#6897=REPRESENTATION('material name',(#6914),#19082);
#6898=REPRESENTATION('density',(#6864),#19082);
#6899=REPRESENTATION('material name',(#6915),#19084);
#6900=REPRESENTATION('density',(#6865),#19084);
#6901=REPRESENTATION('material name',(#6916),#19085);
#6902=REPRESENTATION('density',(#6866),#19085);
#6903=REPRESENTATION('material name',(#6917),#19086);
#6904=REPRESENTATION('density',(#6867),#19086);
#6905=REPRESENTATION('material name',(#6918),#19087);
#6906=REPRESENTATION('density',(#6868),#19087);
#6907=REPRESENTATION('material name',(#6919),#19088);
#6908=REPRESENTATION('density',(#6869),#19088);
#6909=REPRESENTATION('material name',(#6920),#19089);
#6910=REPRESENTATION('density',(#6870),#19089);
#6911=DESCRIPTIVE_REPRESENTATION_ITEM('Steel','Steel');
#6912=DESCRIPTIVE_REPRESENTATION_ITEM('Steel','Steel');
#6913=DESCRIPTIVE_REPRESENTATION_ITEM('Steel','Steel');
#6914=DESCRIPTIVE_REPRESENTATION_ITEM('Steel','Steel');
#6915=DESCRIPTIVE_REPRESENTATION_ITEM('Steel','Steel');
#6916=DESCRIPTIVE_REPRESENTATION_ITEM('Steel','Steel');
#6917=DESCRIPTIVE_REPRESENTATION_ITEM('Steel','Steel');
#6918=DESCRIPTIVE_REPRESENTATION_ITEM('Steel','Steel');
#6919=DESCRIPTIVE_REPRESENTATION_ITEM('Steel','Steel');
#6920=DESCRIPTIVE_REPRESENTATION_ITEM('Steel','Steel');
#6921=PROPERTY_DEFINITION('material property','material name',#19149);
#6922=PROPERTY_DEFINITION('material property','density of part',#19149);
#6923=PROPERTY_DEFINITION('material property','material name',#19150);
#6924=PROPERTY_DEFINITION('material property','density of part',#19150);
#6925=PROPERTY_DEFINITION('material property','material name',#19151);
#6926=PROPERTY_DEFINITION('material property','density of part',#19151);
#6927=PROPERTY_DEFINITION('material property','material name',#19152);
#6928=PROPERTY_DEFINITION('material property','density of part',#19152);
#6929=PROPERTY_DEFINITION('material property','material name',#19154);
#6930=PROPERTY_DEFINITION('material property','density of part',#19154);
#6931=PROPERTY_DEFINITION('material property','material name',#19155);
#6932=PROPERTY_DEFINITION('material property','density of part',#19155);
#6933=PROPERTY_DEFINITION('material property','material name',#19156);
#6934=PROPERTY_DEFINITION('material property','density of part',#19156);
#6935=PROPERTY_DEFINITION('material property','material name',#19157);
#6936=PROPERTY_DEFINITION('material property','density of part',#19157);
#6937=PROPERTY_DEFINITION('material property','material name',#19158);
#6938=PROPERTY_DEFINITION('material property','density of part',#19158);
#6939=PROPERTY_DEFINITION('material property','material name',#19159);
#6940=PROPERTY_DEFINITION('material property','density of part',#19159);
#6941=AXIS2_PLACEMENT_3D('',#8878,#7437,#7438);
#6942=AXIS2_PLACEMENT_3D('',#8879,#7439,#7440);
#6943=AXIS2_PLACEMENT_3D('',#8880,#7441,#7442);
#6944=AXIS2_PLACEMENT_3D('',#8882,#7443,#7444);
#6945=AXIS2_PLACEMENT_3D('',#8885,#7446,#7447);
#6946=AXIS2_PLACEMENT_3D('',#8886,#7448,#7449);
#6947=AXIS2_PLACEMENT_3D('',#8888,#7450,#7451);
#6948=AXIS2_PLACEMENT_3D('',#8891,#7453,#7454);
#6949=AXIS2_PLACEMENT_3D('',#8892,#7455,#7456);
#6950=AXIS2_PLACEMENT_3D('',#8894,#7457,#7458);
#6951=AXIS2_PLACEMENT_3D('',#8897,#7460,#7461);
#6952=AXIS2_PLACEMENT_3D('',#8898,#7462,#7463);
#6953=AXIS2_PLACEMENT_3D('',#8905,#7467,#7468);
#6954=AXIS2_PLACEMENT_3D('',#8911,#7472,#7473);
#6955=AXIS2_PLACEMENT_3D('',#8915,#7476,#7477);
#6956=AXIS2_PLACEMENT_3D('',#8927,#7484,#7485);
#6957=AXIS2_PLACEMENT_3D('',#8931,#7488,#7489);
#6958=AXIS2_PLACEMENT_3D('',#8935,#7492,#7493);
#6959=AXIS2_PLACEMENT_3D('',#8939,#7496,#7497);
#6960=AXIS2_PLACEMENT_3D('',#8941,#7498,#7499);
#6961=AXIS2_PLACEMENT_3D('',#8955,#7506,#7507);
#6962=AXIS2_PLACEMENT_3D('',#8965,#7513,#7514);
#6963=AXIS2_PLACEMENT_3D('',#8971,#7518,#7519);
#6964=AXIS2_PLACEMENT_3D('',#8979,#7524,#7525);
#6965=AXIS2_PLACEMENT_3D('',#8981,#7527,#7528);
#6966=AXIS2_PLACEMENT_3D('',#8987,#7532,#7533);
#6967=AXIS2_PLACEMENT_3D('',#8989,#7535,#7536);
#6968=AXIS2_PLACEMENT_3D('',#8991,#7538,#7539);
#6969=AXIS2_PLACEMENT_3D('',#8993,#7541,#7542);
#6970=AXIS2_PLACEMENT_3D('',#8995,#7543,#7544);
#6971=AXIS2_PLACEMENT_3D('',#9008,#7551,#7552);
#6972=AXIS2_PLACEMENT_3D('',#9009,#7553,#7554);
#6973=AXIS2_PLACEMENT_3D('',#9011,#7556,#7557);
#6974=AXIS2_PLACEMENT_3D('',#9014,#7560,#7561);
#6975=AXIS2_PLACEMENT_3D('',#9016,#7563,#7564);
#6976=AXIS2_PLACEMENT_3D('',#9018,#7566,#7567);
#6977=AXIS2_PLACEMENT_3D('',#9020,#7569,#7570);
#6978=AXIS2_PLACEMENT_3D('',#9022,#7572,#7573);
#6979=AXIS2_PLACEMENT_3D('',#9023,#7574,#7575);
#6980=AXIS2_PLACEMENT_3D('',#9024,#7576,#7577);
#6981=AXIS2_PLACEMENT_3D('',#9025,#7578,#7579);
#6982=AXIS2_PLACEMENT_3D('',#9027,#7580,#7581);
#6983=AXIS2_PLACEMENT_3D('',#9030,#7583,#7584);
#6984=AXIS2_PLACEMENT_3D('',#9031,#7585,#7586);
#6985=AXIS2_PLACEMENT_3D('',#9033,#7587,#7588);
#6986=AXIS2_PLACEMENT_3D('',#9036,#7590,#7591);
#6987=AXIS2_PLACEMENT_3D('',#9037,#7592,#7593);
#6988=AXIS2_PLACEMENT_3D('',#9039,#7594,#7595);
#6989=AXIS2_PLACEMENT_3D('',#9042,#7597,#7598);
#6990=AXIS2_PLACEMENT_3D('',#9043,#7599,#7600);
#6991=AXIS2_PLACEMENT_3D('',#9052,#7605,#7606);
#6992=AXIS2_PLACEMENT_3D('',#9060,#7611,#7612);
#6993=AXIS2_PLACEMENT_3D('',#9068,#7617,#7618);
#6994=AXIS2_PLACEMENT_3D('',#9077,#7623,#7624);
#6995=AXIS2_PLACEMENT_3D('',#9081,#7627,#7628);
#6996=AXIS2_PLACEMENT_3D('',#9085,#7631,#7632);
#6997=AXIS2_PLACEMENT_3D('',#9088,#7635,#7636);
#6998=AXIS2_PLACEMENT_3D('',#9090,#7637,#7638);
#6999=AXIS2_PLACEMENT_3D('',#9103,#7645,#7646);
#7000=AXIS2_PLACEMENT_3D('',#9104,#7647,#7648);
#7001=AXIS2_PLACEMENT_3D('',#9106,#7649,#7650);
#7002=AXIS2_PLACEMENT_3D('',#9108,#7652,#7653);
#7003=AXIS2_PLACEMENT_3D('',#9114,#7657,#7658);
#7004=AXIS2_PLACEMENT_3D('',#9118,#7661,#7662);
#7005=AXIS2_PLACEMENT_3D('',#9122,#7665,#7666);
#7006=AXIS2_PLACEMENT_3D('',#9126,#7669,#7670);
#7007=AXIS2_PLACEMENT_3D('',#9130,#7673,#7674);
#7008=AXIS2_PLACEMENT_3D('',#9132,#7676,#7677);
#7009=AXIS2_PLACEMENT_3D('',#9133,#7678,#7679);
#7010=AXIS2_PLACEMENT_3D('',#9134,#7680,#7681);
#7011=AXIS2_PLACEMENT_3D('',#9135,#7682,#7683);
#7012=AXIS2_PLACEMENT_3D('',#9136,#7684,#7685);
#7013=AXIS2_PLACEMENT_3D('',#9138,#7686,#7687);
#7014=AXIS2_PLACEMENT_3D('',#9141,#7689,#7690);
#7015=AXIS2_PLACEMENT_3D('',#9142,#7691,#7692);
#7016=AXIS2_PLACEMENT_3D('',#9144,#7693,#7694);
#7017=AXIS2_PLACEMENT_3D('',#9145,#7695,#7696);
#7018=AXIS2_PLACEMENT_3D('',#9147,#7697,#7698);
#7019=AXIS2_PLACEMENT_3D('',#9148,#7699,#7700);
#7020=AXIS2_PLACEMENT_3D('',#9150,#7701,#7702);
#7021=AXIS2_PLACEMENT_3D('',#9152,#7704,#7705);
#7022=AXIS2_PLACEMENT_3D('',#9154,#7706,#7707);
#7023=AXIS2_PLACEMENT_3D('',#9156,#7708,#7709);
#7024=AXIS2_PLACEMENT_3D('',#9157,#7710,#7711);
#7025=AXIS2_PLACEMENT_3D('',#9160,#7713,#7714);
#7026=AXIS2_PLACEMENT_3D('',#9161,#7715,#7716);
#7027=AXIS2_PLACEMENT_3D('',#9162,#7717,#7718);
#7028=AXIS2_PLACEMENT_3D('',#9164,#7720,#7721);
#7029=AXIS2_PLACEMENT_3D('',#9165,#7722,#7723);
#7030=AXIS2_PLACEMENT_3D('',#9166,#7724,#7725);
#7031=AXIS2_PLACEMENT_3D('',#9175,#7730,#7731);
#7032=AXIS2_PLACEMENT_3D('',#9184,#7736,#7737);
#7033=AXIS2_PLACEMENT_3D('',#9185,#7738,#7739);
#7034=AXIS2_PLACEMENT_3D('',#9186,#7740,#7741);
#7035=AXIS2_PLACEMENT_3D('',#9187,#7742,#7743);
#7036=AXIS2_PLACEMENT_3D('',#9188,#7744,#7745);
#7037=AXIS2_PLACEMENT_3D('',#9189,#7746,#7747);
#7038=AXIS2_PLACEMENT_3D('',#9190,#7748,#7749);
#7039=AXIS2_PLACEMENT_3D('',#9191,#7750,#7751);
#7040=AXIS2_PLACEMENT_3D('',#9192,#7752,#7753);
#7041=AXIS2_PLACEMENT_3D('',#9193,#7754,#7755);
#7042=AXIS2_PLACEMENT_3D('',#9194,#7756,#7757);
#7043=AXIS2_PLACEMENT_3D('',#9260,#7760,#7761);
#7044=AXIS2_PLACEMENT_3D('',#9262,#7762,#7763);
#7045=AXIS2_PLACEMENT_3D('',#9264,#7764,#7765);
#7046=AXIS2_PLACEMENT_3D('',#9265,#7766,#7767);
#7047=AXIS2_PLACEMENT_3D('',#9267,#7768,#7769);
#7048=AXIS2_PLACEMENT_3D('',#9270,#7771,#7772);
#7049=AXIS2_PLACEMENT_3D('',#9271,#7773,#7774);
#7050=AXIS2_PLACEMENT_3D('',#9273,#7775,#7776);
#7051=AXIS2_PLACEMENT_3D('',#9275,#7778,#7779);
#7052=AXIS2_PLACEMENT_3D('',#9277,#7780,#7781);
#7053=AXIS2_PLACEMENT_3D('',#9279,#7783,#7784);
#7054=AXIS2_PLACEMENT_3D('',#9281,#7785,#7786);
#7055=AXIS2_PLACEMENT_3D('',#9284,#7788,#7789);
#7056=AXIS2_PLACEMENT_3D('',#9285,#7790,#7791);
#7057=AXIS2_PLACEMENT_3D('',#9287,#7792,#7793);
#7058=AXIS2_PLACEMENT_3D('',#9290,#7795,#7796);
#7059=AXIS2_PLACEMENT_3D('',#9291,#7797,#7798);
#7060=AXIS2_PLACEMENT_3D('',#9293,#7799,#7800);
#7061=AXIS2_PLACEMENT_3D('',#9294,#7801,#7802);
#7062=AXIS2_PLACEMENT_3D('',#9296,#7803,#7804);
#7063=AXIS2_PLACEMENT_3D('',#9299,#7806,#7807);
#7064=AXIS2_PLACEMENT_3D('',#9300,#7808,#7809);
#7065=AXIS2_PLACEMENT_3D('',#9302,#7810,#7811);
#7066=AXIS2_PLACEMENT_3D('',#9303,#7812,#7813);
#7067=AXIS2_PLACEMENT_3D('',#9306,#7815,#7816);
#7068=AXIS2_PLACEMENT_3D('',#9307,#7817,#7818);
#7069=AXIS2_PLACEMENT_3D('',#9310,#7820,#7821);
#7070=AXIS2_PLACEMENT_3D('',#9311,#7822,#7823);
#7071=AXIS2_PLACEMENT_3D('',#9320,#7828,#7829);
#7072=AXIS2_PLACEMENT_3D('',#9329,#7834,#7835);
#7073=AXIS2_PLACEMENT_3D('',#9338,#7840,#7841);
#7074=AXIS2_PLACEMENT_3D('',#9347,#7846,#7847);
#7075=AXIS2_PLACEMENT_3D('',#9356,#7852,#7853);
#7076=AXIS2_PLACEMENT_3D('',#9365,#7858,#7859);
#7077=AXIS2_PLACEMENT_3D('',#9374,#7864,#7865);
#7078=AXIS2_PLACEMENT_3D('',#9376,#7866,#7867);
#7079=AXIS2_PLACEMENT_3D('',#9377,#7868,#7869);
#7080=AXIS2_PLACEMENT_3D('',#9379,#7870,#7871);
#7081=AXIS2_PLACEMENT_3D('',#9380,#7872,#7873);
#7082=AXIS2_PLACEMENT_3D('',#9383,#7876,#7877);
#7083=AXIS2_PLACEMENT_3D('',#9386,#7880,#7881);
#7084=AXIS2_PLACEMENT_3D('',#9389,#7884,#7885);
#7085=AXIS2_PLACEMENT_3D('',#9395,#7889,#7890);
#7086=AXIS2_PLACEMENT_3D('',#9401,#7894,#7895);
#7087=AXIS2_PLACEMENT_3D('',#9478,#7898,#7899);
#7088=AXIS2_PLACEMENT_3D('',#9556,#7903,#7904);
#7089=AXIS2_PLACEMENT_3D('',#9634,#7908,#7909);
#7090=AXIS2_PLACEMENT_3D('',#9709,#7912,#7913);
#7091=AXIS2_PLACEMENT_3D('',#9725,#7917,#7918);
#7092=AXIS2_PLACEMENT_3D('',#10103,#7930,#7931);
#7093=AXIS2_PLACEMENT_3D('',#10105,#7932,#7933);
#7094=AXIS2_PLACEMENT_3D('',#10107,#7935,#7936);
#7095=AXIS2_PLACEMENT_3D('',#10109,#7938,#7939);
#7096=AXIS2_PLACEMENT_3D('',#10277,#7941,#7942);
#7097=AXIS2_PLACEMENT_3D('',#10278,#7943,#7944);
#7098=AXIS2_PLACEMENT_3D('',#10283,#7945,#7946);
#7099=AXIS2_PLACEMENT_3D('',#10355,#7948,#7949);
#7100=AXIS2_PLACEMENT_3D('',#10473,#7951,#7952);
#7101=AXIS2_PLACEMENT_3D('',#10518,#7953,#7954);
#7102=AXIS2_PLACEMENT_3D('',#10669,#7955,#7956);
#7103=AXIS2_PLACEMENT_3D('',#10789,#7958,#7959);
#7104=AXIS2_PLACEMENT_3D('',#10794,#7960,#7961);
#7105=AXIS2_PLACEMENT_3D('',#10846,#7963,#7964);
#7106=AXIS2_PLACEMENT_3D('',#10847,#7965,#7966);
#7107=AXIS2_PLACEMENT_3D('',#10848,#7967,#7968);
#7108=AXIS2_PLACEMENT_3D('',#10849,#7969,#7970);
#7109=AXIS2_PLACEMENT_3D('',#10850,#7971,#7972);
#7110=AXIS2_PLACEMENT_3D('',#10851,#7973,#7974);
#7111=AXIS2_PLACEMENT_3D('',#10853,#7975,#7976);
#7112=AXIS2_PLACEMENT_3D('',#10854,#7977,#7978);
#7113=AXIS2_PLACEMENT_3D('',#10855,#7979,#7980);
#7114=AXIS2_PLACEMENT_3D('',#10856,#7981,#7982);
#7115=AXIS2_PLACEMENT_3D('',#10857,#7983,#7984);
#7116=AXIS2_PLACEMENT_3D('',#10858,#7985,#7986);
#7117=AXIS2_PLACEMENT_3D('',#10879,#7987,#7988);
#7118=AXIS2_PLACEMENT_3D('',#10881,#7989,#7990);
#7119=AXIS2_PLACEMENT_3D('',#10882,#7991,#7992);
#7120=AXIS2_PLACEMENT_3D('',#10883,#7993,#7994);
#7121=AXIS2_PLACEMENT_3D('',#10981,#7996,#7997);
#7122=AXIS2_PLACEMENT_3D('',#10982,#7998,#7999);
#7123=AXIS2_PLACEMENT_3D('',#10985,#8000,#8001);
#7124=AXIS2_PLACEMENT_3D('',#10987,#8002,#8003);
#7125=AXIS2_PLACEMENT_3D('',#10988,#8004,#8005);
#7126=AXIS2_PLACEMENT_3D('',#10989,#8006,#8007);
#7127=AXIS2_PLACEMENT_3D('',#10992,#8008,#8009);
#7128=AXIS2_PLACEMENT_3D('',#10994,#8010,#8011);
#7129=AXIS2_PLACEMENT_3D('',#10995,#8012,#8013);
#7130=AXIS2_PLACEMENT_3D('',#10996,#8014,#8015);
#7131=AXIS2_PLACEMENT_3D('',#10999,#8016,#8017);
#7132=AXIS2_PLACEMENT_3D('',#11001,#8018,#8019);
#7133=AXIS2_PLACEMENT_3D('',#11002,#8020,#8021);
#7134=AXIS2_PLACEMENT_3D('',#11003,#8022,#8023);
#7135=AXIS2_PLACEMENT_3D('',#11034,#8026,#8027);
#7136=AXIS2_PLACEMENT_3D('',#11037,#8028,#8029);
#7137=AXIS2_PLACEMENT_3D('',#11039,#8030,#8031);
#7138=AXIS2_PLACEMENT_3D('',#11040,#8032,#8033);
#7139=AXIS2_PLACEMENT_3D('',#11041,#8034,#8035);
#7140=AXIS2_PLACEMENT_3D('',#11222,#8038,#8039);
#7141=AXIS2_PLACEMENT_3D('',#11223,#8040,#8041);
#7142=AXIS2_PLACEMENT_3D('',#11240,#8042,#8043);
#7143=AXIS2_PLACEMENT_3D('',#11241,#8044,#8045);
#7144=AXIS2_PLACEMENT_3D('',#11242,#8046,#8047);
#7145=AXIS2_PLACEMENT_3D('',#11308,#8050,#8051);
#7146=AXIS2_PLACEMENT_3D('',#11310,#8052,#8053);
#7147=AXIS2_PLACEMENT_3D('',#11312,#8054,#8055);
#7148=AXIS2_PLACEMENT_3D('',#11313,#8056,#8057);
#7149=AXIS2_PLACEMENT_3D('',#11315,#8058,#8059);
#7150=AXIS2_PLACEMENT_3D('',#11318,#8061,#8062);
#7151=AXIS2_PLACEMENT_3D('',#11319,#8063,#8064);
#7152=AXIS2_PLACEMENT_3D('',#11321,#8065,#8066);
#7153=AXIS2_PLACEMENT_3D('',#11323,#8068,#8069);
#7154=AXIS2_PLACEMENT_3D('',#11325,#8070,#8071);
#7155=AXIS2_PLACEMENT_3D('',#11327,#8073,#8074);
#7156=AXIS2_PLACEMENT_3D('',#11329,#8075,#8076);
#7157=AXIS2_PLACEMENT_3D('',#11332,#8078,#8079);
#7158=AXIS2_PLACEMENT_3D('',#11333,#8080,#8081);
#7159=AXIS2_PLACEMENT_3D('',#11342,#8086,#8087);
#7160=AXIS2_PLACEMENT_3D('',#11348,#8091,#8092);
#7161=AXIS2_PLACEMENT_3D('',#11354,#8096,#8097);
#7162=AXIS2_PLACEMENT_3D('',#11360,#8101,#8102);
#7163=AXIS2_PLACEMENT_3D('',#11366,#8106,#8107);
#7164=AXIS2_PLACEMENT_3D('',#11369,#8110,#8111);
#7165=AXIS2_PLACEMENT_3D('',#11371,#8112,#8113);
#7166=AXIS2_PLACEMENT_3D('',#11372,#8114,#8115);
#7167=AXIS2_PLACEMENT_3D('',#11381,#8120,#8121);
#7168=AXIS2_PLACEMENT_3D('',#11387,#8125,#8126);
#7169=AXIS2_PLACEMENT_3D('',#11393,#8130,#8131);
#7170=AXIS2_PLACEMENT_3D('',#11399,#8135,#8136);
#7171=AXIS2_PLACEMENT_3D('',#11405,#8140,#8141);
#7172=AXIS2_PLACEMENT_3D('',#11408,#8144,#8145);
#7173=AXIS2_PLACEMENT_3D('',#11410,#8146,#8147);
#7174=AXIS2_PLACEMENT_3D('',#11411,#8148,#8149);
#7175=AXIS2_PLACEMENT_3D('',#11414,#8151,#8152);
#7176=AXIS2_PLACEMENT_3D('',#11415,#8153,#8154);
#7177=AXIS2_PLACEMENT_3D('',#11418,#8156,#8157);
#7178=AXIS2_PLACEMENT_3D('',#11419,#8158,#8159);
#7179=AXIS2_PLACEMENT_3D('',#11428,#8164,#8165);
#7180=AXIS2_PLACEMENT_3D('',#11437,#8170,#8171);
#7181=AXIS2_PLACEMENT_3D('',#11446,#8176,#8177);
#7182=AXIS2_PLACEMENT_3D('',#11455,#8182,#8183);
#7183=AXIS2_PLACEMENT_3D('',#11464,#8188,#8189);
#7184=AXIS2_PLACEMENT_3D('',#11473,#8194,#8195);
#7185=AXIS2_PLACEMENT_3D('',#11482,#8200,#8201);
#7186=AXIS2_PLACEMENT_3D('',#11484,#8202,#8203);
#7187=AXIS2_PLACEMENT_3D('',#11485,#8204,#8205);
#7188=AXIS2_PLACEMENT_3D('',#11487,#8206,#8207);
#7189=AXIS2_PLACEMENT_3D('',#11488,#8208,#8209);
#7190=AXIS2_PLACEMENT_3D('',#11491,#8212,#8213);
#7191=AXIS2_PLACEMENT_3D('',#11494,#8216,#8217);
#7192=AXIS2_PLACEMENT_3D('',#11497,#8220,#8221);
#7193=AXIS2_PLACEMENT_3D('',#11503,#8225,#8226);
#7194=AXIS2_PLACEMENT_3D('',#11509,#8230,#8231);
#7195=AXIS2_PLACEMENT_3D('',#11586,#8234,#8235);
#7196=AXIS2_PLACEMENT_3D('',#11664,#8239,#8240);
#7197=AXIS2_PLACEMENT_3D('',#11742,#8244,#8245);
#7198=AXIS2_PLACEMENT_3D('',#11817,#8248,#8249);
#7199=AXIS2_PLACEMENT_3D('',#11833,#8253,#8254);
#7200=AXIS2_PLACEMENT_3D('',#12211,#8266,#8267);
#7201=AXIS2_PLACEMENT_3D('',#12213,#8268,#8269);
#7202=AXIS2_PLACEMENT_3D('',#12215,#8271,#8272);
#7203=AXIS2_PLACEMENT_3D('',#12217,#8274,#8275);
#7204=AXIS2_PLACEMENT_3D('',#12385,#8277,#8278);
#7205=AXIS2_PLACEMENT_3D('',#12386,#8279,#8280);
#7206=AXIS2_PLACEMENT_3D('',#12391,#8281,#8282);
#7207=AXIS2_PLACEMENT_3D('',#12463,#8284,#8285);
#7208=AXIS2_PLACEMENT_3D('',#12581,#8287,#8288);
#7209=AXIS2_PLACEMENT_3D('',#12626,#8289,#8290);
#7210=AXIS2_PLACEMENT_3D('',#12777,#8291,#8292);
#7211=AXIS2_PLACEMENT_3D('',#12897,#8294,#8295);
#7212=AXIS2_PLACEMENT_3D('',#12902,#8296,#8297);
#7213=AXIS2_PLACEMENT_3D('',#12954,#8299,#8300);
#7214=AXIS2_PLACEMENT_3D('',#12955,#8301,#8302);
#7215=AXIS2_PLACEMENT_3D('',#12956,#8303,#8304);
#7216=AXIS2_PLACEMENT_3D('',#12957,#8305,#8306);
#7217=AXIS2_PLACEMENT_3D('',#12958,#8307,#8308);
#7218=AXIS2_PLACEMENT_3D('',#12959,#8309,#8310);
#7219=AXIS2_PLACEMENT_3D('',#12961,#8311,#8312);
#7220=AXIS2_PLACEMENT_3D('',#12962,#8313,#8314);
#7221=AXIS2_PLACEMENT_3D('',#12963,#8315,#8316);
#7222=AXIS2_PLACEMENT_3D('',#12964,#8317,#8318);
#7223=AXIS2_PLACEMENT_3D('',#12965,#8319,#8320);
#7224=AXIS2_PLACEMENT_3D('',#12966,#8321,#8322);
#7225=AXIS2_PLACEMENT_3D('',#12987,#8323,#8324);
#7226=AXIS2_PLACEMENT_3D('',#12989,#8325,#8326);
#7227=AXIS2_PLACEMENT_3D('',#12990,#8327,#8328);
#7228=AXIS2_PLACEMENT_3D('',#12991,#8329,#8330);
#7229=AXIS2_PLACEMENT_3D('',#13089,#8332,#8333);
#7230=AXIS2_PLACEMENT_3D('',#13090,#8334,#8335);
#7231=AXIS2_PLACEMENT_3D('',#13093,#8336,#8337);
#7232=AXIS2_PLACEMENT_3D('',#13095,#8338,#8339);
#7233=AXIS2_PLACEMENT_3D('',#13096,#8340,#8341);
#7234=AXIS2_PLACEMENT_3D('',#13097,#8342,#8343);
#7235=AXIS2_PLACEMENT_3D('',#13100,#8344,#8345);
#7236=AXIS2_PLACEMENT_3D('',#13102,#8346,#8347);
#7237=AXIS2_PLACEMENT_3D('',#13103,#8348,#8349);
#7238=AXIS2_PLACEMENT_3D('',#13104,#8350,#8351);
#7239=AXIS2_PLACEMENT_3D('',#13107,#8352,#8353);
#7240=AXIS2_PLACEMENT_3D('',#13109,#8354,#8355);
#7241=AXIS2_PLACEMENT_3D('',#13110,#8356,#8357);
#7242=AXIS2_PLACEMENT_3D('',#13111,#8358,#8359);
#7243=AXIS2_PLACEMENT_3D('',#13142,#8362,#8363);
#7244=AXIS2_PLACEMENT_3D('',#13145,#8364,#8365);
#7245=AXIS2_PLACEMENT_3D('',#13147,#8366,#8367);
#7246=AXIS2_PLACEMENT_3D('',#13148,#8368,#8369);
#7247=AXIS2_PLACEMENT_3D('',#13149,#8370,#8371);
#7248=AXIS2_PLACEMENT_3D('',#13330,#8374,#8375);
#7249=AXIS2_PLACEMENT_3D('',#13331,#8376,#8377);
#7250=AXIS2_PLACEMENT_3D('',#13348,#8378,#8379);
#7251=AXIS2_PLACEMENT_3D('',#13349,#8380,#8381);
#7252=AXIS2_PLACEMENT_3D('',#13350,#8382,#8383);
#7253=AXIS2_PLACEMENT_3D('',#13352,#8384,#8385);
#7254=AXIS2_PLACEMENT_3D('',#13355,#8387,#8388);
#7255=AXIS2_PLACEMENT_3D('',#13356,#8389,#8390);
#7256=AXIS2_PLACEMENT_3D('',#13358,#8391,#8392);
#7257=AXIS2_PLACEMENT_3D('',#13361,#8394,#8395);
#7258=AXIS2_PLACEMENT_3D('',#13362,#8396,#8397);
#7259=AXIS2_PLACEMENT_3D('',#13364,#8398,#8399);
#7260=AXIS2_PLACEMENT_3D('',#13366,#8400,#8401);
#7261=AXIS2_PLACEMENT_3D('',#13367,#8402,#8403);
#7262=AXIS2_PLACEMENT_3D('',#13369,#8404,#8405);
#7263=AXIS2_PLACEMENT_3D('',#13371,#8407,#8408);
#7264=AXIS2_PLACEMENT_3D('',#13372,#8409,#8410);
#7265=AXIS2_PLACEMENT_3D('',#13374,#8411,#8412);
#7266=AXIS2_PLACEMENT_3D('',#13376,#8413,#8414);
#7267=AXIS2_PLACEMENT_3D('',#13377,#8415,#8416);
#7268=AXIS2_PLACEMENT_3D('',#13379,#8417,#8418);
#7269=AXIS2_PLACEMENT_3D('',#13381,#8420,#8421);
#7270=AXIS2_PLACEMENT_3D('',#13382,#8422,#8423);
#7271=AXIS2_PLACEMENT_3D('',#13384,#8424,#8425);
#7272=AXIS2_PLACEMENT_3D('',#13386,#8426,#8427);
#7273=AXIS2_PLACEMENT_3D('',#13387,#8428,#8429);
#7274=AXIS2_PLACEMENT_3D('',#13389,#8430,#8431);
#7275=AXIS2_PLACEMENT_3D('',#13391,#8433,#8434);
#7276=AXIS2_PLACEMENT_3D('',#13392,#8435,#8436);
#7277=AXIS2_PLACEMENT_3D('',#13394,#8437,#8438);
#7278=AXIS2_PLACEMENT_3D('',#13396,#8439,#8440);
#7279=AXIS2_PLACEMENT_3D('',#13397,#8441,#8442);
#7280=AXIS2_PLACEMENT_3D('',#13399,#8443,#8444);
#7281=AXIS2_PLACEMENT_3D('',#13401,#8446,#8447);
#7282=AXIS2_PLACEMENT_3D('',#13402,#8448,#8449);
#7283=AXIS2_PLACEMENT_3D('',#13405,#8451,#8452);
#7284=AXIS2_PLACEMENT_3D('',#13406,#8453,#8454);
#7285=AXIS2_PLACEMENT_3D('',#13409,#8456,#8457);
#7286=AXIS2_PLACEMENT_3D('',#13410,#8458,#8459);
#7287=AXIS2_PLACEMENT_3D('',#13413,#8461,#8462);
#7288=AXIS2_PLACEMENT_3D('',#13414,#8463,#8464);
#7289=AXIS2_PLACEMENT_3D('',#13417,#8466,#8467);
#7290=AXIS2_PLACEMENT_3D('',#13445,#8468,#8469);
#7291=AXIS2_PLACEMENT_3D('',#13453,#8470,#8471);
#7292=AXIS2_PLACEMENT_3D('',#13459,#8472,#8473);
#7293=AXIS2_PLACEMENT_3D('',#13462,#8474,#8475);
#7294=AXIS2_PLACEMENT_3D('',#13492,#8478,#8479);
#7295=AXIS2_PLACEMENT_3D('',#13530,#8480,#8481);
#7296=AXIS2_PLACEMENT_3D('',#13568,#8482,#8483);
#7297=AXIS2_PLACEMENT_3D('',#13579,#8484,#8485);
#7298=AXIS2_PLACEMENT_3D('',#13582,#8486,#8487);
#7299=AXIS2_PLACEMENT_3D('',#13612,#8490,#8491);
#7300=AXIS2_PLACEMENT_3D('',#13658,#8492,#8493);
#7301=AXIS2_PLACEMENT_3D('',#13811,#8495,#8496);
#7302=AXIS2_PLACEMENT_3D('',#13812,#8497,#8498);
#7303=AXIS2_PLACEMENT_3D('',#13935,#8500,#8501);
#7304=AXIS2_PLACEMENT_3D('',#13956,#8502,#8503);
#7305=AXIS2_PLACEMENT_3D('',#13957,#8504,#8505);
#7306=AXIS2_PLACEMENT_3D('',#13973,#8507,#8508);
#7307=AXIS2_PLACEMENT_3D('',#13981,#8509,#8510);
#7308=AXIS2_PLACEMENT_3D('',#14029,#8512,#8513);
#7309=AXIS2_PLACEMENT_3D('',#14077,#8515,#8516);
#7310=AXIS2_PLACEMENT_3D('',#14128,#8518,#8519);
#7311=AXIS2_PLACEMENT_3D('',#14176,#8521,#8522);
#7312=AXIS2_PLACEMENT_3D('',#14224,#8524,#8525);
#7313=AXIS2_PLACEMENT_3D('',#14272,#8527,#8528);
#7314=AXIS2_PLACEMENT_3D('',#14326,#8530,#8531);
#7315=AXIS2_PLACEMENT_3D('',#14374,#8533,#8534);
#7316=AXIS2_PLACEMENT_3D('',#14422,#8536,#8537);
#7317=AXIS2_PLACEMENT_3D('',#14476,#8539,#8540);
#7318=AXIS2_PLACEMENT_3D('',#14524,#8542,#8543);
#7319=AXIS2_PLACEMENT_3D('',#14572,#8545,#8546);
#7320=AXIS2_PLACEMENT_3D('',#14620,#8548,#8549);
#7321=AXIS2_PLACEMENT_3D('',#14674,#8551,#8552);
#7322=AXIS2_PLACEMENT_3D('',#14722,#8554,#8555);
#7323=AXIS2_PLACEMENT_3D('',#14770,#8557,#8558);
#7324=AXIS2_PLACEMENT_3D('',#14824,#8560,#8561);
#7325=AXIS2_PLACEMENT_3D('',#14872,#8563,#8564);
#7326=AXIS2_PLACEMENT_3D('',#14920,#8566,#8567);
#7327=AXIS2_PLACEMENT_3D('',#14974,#8569,#8570);
#7328=AXIS2_PLACEMENT_3D('',#15022,#8572,#8573);
#7329=AXIS2_PLACEMENT_3D('',#15070,#8575,#8576);
#7330=AXIS2_PLACEMENT_3D('',#15118,#8578,#8579);
#7331=AXIS2_PLACEMENT_3D('',#15172,#8581,#8582);
#7332=AXIS2_PLACEMENT_3D('',#15220,#8584,#8585);
#7333=AXIS2_PLACEMENT_3D('',#15268,#8587,#8588);
#7334=AXIS2_PLACEMENT_3D('',#15322,#8590,#8591);
#7335=AXIS2_PLACEMENT_3D('',#15370,#8593,#8594);
#7336=AXIS2_PLACEMENT_3D('',#15418,#8596,#8597);
#7337=AXIS2_PLACEMENT_3D('',#15434,#8599,#8600);
#7338=AXIS2_PLACEMENT_3D('',#15444,#8601,#8602);
#7339=AXIS2_PLACEMENT_3D('',#15468,#8604,#8605);
#7340=AXIS2_PLACEMENT_3D('',#15492,#8607,#8608);
#7341=AXIS2_PLACEMENT_3D('',#15517,#8610,#8611);
#7342=AXIS2_PLACEMENT_3D('',#15542,#8613,#8614);
#7343=AXIS2_PLACEMENT_3D('',#15566,#8616,#8617);
#7344=AXIS2_PLACEMENT_3D('',#15591,#8619,#8620);
#7345=AXIS2_PLACEMENT_3D('',#15616,#8622,#8623);
#7346=AXIS2_PLACEMENT_3D('',#15640,#8625,#8626);
#7347=AXIS2_PLACEMENT_3D('',#15664,#8628,#8629);
#7348=AXIS2_PLACEMENT_3D('',#15689,#8631,#8632);
#7349=AXIS2_PLACEMENT_3D('',#15714,#8634,#8635);
#7350=AXIS2_PLACEMENT_3D('',#15738,#8637,#8638);
#7351=AXIS2_PLACEMENT_3D('',#15763,#8640,#8641);
#7352=AXIS2_PLACEMENT_3D('',#15788,#8643,#8644);
#7353=AXIS2_PLACEMENT_3D('',#15812,#8646,#8647);
#7354=AXIS2_PLACEMENT_3D('',#15837,#8649,#8650);
#7355=AXIS2_PLACEMENT_3D('',#15862,#8652,#8653);
#7356=AXIS2_PLACEMENT_3D('',#15886,#8655,#8656);
#7357=AXIS2_PLACEMENT_3D('',#15910,#8658,#8659);
#7358=AXIS2_PLACEMENT_3D('',#15935,#8661,#8662);
#7359=AXIS2_PLACEMENT_3D('',#15960,#8664,#8665);
#7360=AXIS2_PLACEMENT_3D('',#15984,#8667,#8668);
#7361=AXIS2_PLACEMENT_3D('',#16009,#8670,#8671);
#7362=AXIS2_PLACEMENT_3D('',#16034,#8673,#8674);
#7363=AXIS2_PLACEMENT_3D('',#16058,#8676,#8677);
#7364=AXIS2_PLACEMENT_3D('',#16083,#8679,#8680);
#7365=AXIS2_PLACEMENT_3D('',#16107,#8682,#8683);
#7366=AXIS2_PLACEMENT_3D('',#16132,#8685,#8686);
#7367=AXIS2_PLACEMENT_3D('',#16156,#8688,#8689);
#7368=AXIS2_PLACEMENT_3D('',#16318,#8690,#8691);
#7369=AXIS2_PLACEMENT_3D('',#16337,#8693,#8694);
#7370=AXIS2_PLACEMENT_3D('',#17199,#8695,#8696);
#7371=AXIS2_PLACEMENT_3D('',#17210,#8697,#8698);
#7372=AXIS2_PLACEMENT_3D('',#18077,#8699,#8700);
#7373=AXIS2_PLACEMENT_3D('',#18078,#8701,#8702);
#7374=AXIS2_PLACEMENT_3D('',#18087,#8707,#8708);
#7375=AXIS2_PLACEMENT_3D('',#18093,#8712,#8713);
#7376=AXIS2_PLACEMENT_3D('',#18099,#8717,#8718);
#7377=AXIS2_PLACEMENT_3D('',#18105,#8722,#8723);
#7378=AXIS2_PLACEMENT_3D('',#18111,#8727,#8728);
#7379=AXIS2_PLACEMENT_3D('',#18114,#8731,#8732);
#7380=AXIS2_PLACEMENT_3D('',#18115,#8733,#8734);
#7381=AXIS2_PLACEMENT_3D('',#18117,#8735,#8736);
#7382=AXIS2_PLACEMENT_3D('',#18118,#8737,#8738);
#7383=AXIS2_PLACEMENT_3D('',#18121,#8740,#8741);
#7384=AXIS2_PLACEMENT_3D('',#18122,#8742,#8743);
#7385=AXIS2_PLACEMENT_3D('',#18123,#8744,#8745);
#7386=AXIS2_PLACEMENT_3D('',#18124,#8746,#8747);
#7387=AXIS2_PLACEMENT_3D('',#18125,#8748,#8749);
#7388=AXIS2_PLACEMENT_3D('',#18130,#8751,#8752);
#7389=AXIS2_PLACEMENT_3D('',#18138,#8753,#8754);
#7390=AXIS2_PLACEMENT_3D('',#18162,#8756,#8757);
#7391=AXIS2_PLACEMENT_3D('',#18185,#8758,#8759);
#7392=AXIS2_PLACEMENT_3D('',#18239,#8761,#8762);
#7393=AXIS2_PLACEMENT_3D('',#18287,#8764,#8765);
#7394=AXIS2_PLACEMENT_3D('',#18306,#8767,#8768);
#7395=AXIS2_PLACEMENT_3D('',#18326,#8769,#8770);
#7396=AXIS2_PLACEMENT_3D('',#18339,#8772,#8773);
#7397=AXIS2_PLACEMENT_3D('',#18347,#8774,#8775);
#7398=AXIS2_PLACEMENT_3D('',#18372,#8777,#8778);
#7399=AXIS2_PLACEMENT_3D('',#18397,#8780,#8781);
#7400=AXIS2_PLACEMENT_3D('',#18422,#8783,#8784);
#7401=AXIS2_PLACEMENT_3D('',#18433,#8786,#8787);
#7402=AXIS2_PLACEMENT_3D('',#18439,#8788,#8789);
#7403=AXIS2_PLACEMENT_3D('',#18995,#8790,#8791);
#7404=AXIS2_PLACEMENT_3D('',#19008,#8798,#8799);
#7405=AXIS2_PLACEMENT_3D('',#19009,#8800,#8801);
#7406=AXIS2_PLACEMENT_3D('',#19015,#8805,#8806);
#7407=AXIS2_PLACEMENT_3D('',#19019,#8809,#8810);
#7408=AXIS2_PLACEMENT_3D('',#19023,#8813,#8814);
#7409=AXIS2_PLACEMENT_3D('',#19027,#8817,#8818);
#7410=AXIS2_PLACEMENT_3D('',#19031,#8821,#8822);
#7411=AXIS2_PLACEMENT_3D('',#19033,#8824,#8825);
#7412=AXIS2_PLACEMENT_3D('',#19034,#8826,#8827);
#7413=AXIS2_PLACEMENT_3D('',#19035,#8828,#8829);
#7414=AXIS2_PLACEMENT_3D('',#19036,#8830,#8831);
#7415=AXIS2_PLACEMENT_3D('',#19037,#8832,#8833);
#7416=AXIS2_PLACEMENT_3D('',#19038,#8834,#8835);
#7417=AXIS2_PLACEMENT_3D('',#19039,#8836,#8837);
#7418=AXIS2_PLACEMENT_3D('',#19040,#8838,#8839);
#7419=AXIS2_PLACEMENT_3D('',#19041,#8840,#8841);
#7420=AXIS2_PLACEMENT_3D('',#19042,#8842,#8843);
#7421=AXIS2_PLACEMENT_3D('',#19043,#8844,#8845);
#7422=AXIS2_PLACEMENT_3D('',#19045,#8846,#8847);
#7423=AXIS2_PLACEMENT_3D('',#19048,#8849,#8850);
#7424=AXIS2_PLACEMENT_3D('',#19049,#8851,#8852);
#7425=AXIS2_PLACEMENT_3D('',#19051,#8853,#8854);
#7426=AXIS2_PLACEMENT_3D('',#19054,#8856,#8857);
#7427=AXIS2_PLACEMENT_3D('',#19055,#8858,#8859);
#7428=AXIS2_PLACEMENT_3D('',#19056,#8860,#8861);
#7429=AXIS2_PLACEMENT_3D('',#19057,#8862,#8863);
#7430=AXIS2_PLACEMENT_3D('',#19058,#8864,#8865);
#7431=AXIS2_PLACEMENT_3D('',#19059,#8866,#8867);
#7432=AXIS2_PLACEMENT_3D('',#19060,#8868,#8869);
#7433=AXIS2_PLACEMENT_3D('',#19061,#8870,#8871);
#7434=AXIS2_PLACEMENT_3D('',#19062,#8872,#8873);
#7435=AXIS2_PLACEMENT_3D('',#19063,#8874,#8875);
#7436=AXIS2_PLACEMENT_3D('',#19064,#8876,#8877);
#7437=DIRECTION('axis',(0.,0.,1.));
#7438=DIRECTION('refdir',(1.,0.,0.));
#7439=DIRECTION('axis',(0.,0.,1.));
#7440=DIRECTION('refdir',(1.,0.,0.));
#7441=DIRECTION('center_axis',(0.,0.,-1.));
#7442=DIRECTION('ref_axis',(1.,0.,0.));
#7443=DIRECTION('center_axis',(0.,0.,-1.));
#7444=DIRECTION('ref_axis',(1.,0.,0.));
#7445=DIRECTION('',(0.,0.,-1.));
#7446=DIRECTION('center_axis',(0.,0.,1.));
#7447=DIRECTION('ref_axis',(1.,0.,0.));
#7448=DIRECTION('center_axis',(0.,0.,-1.));
#7449=DIRECTION('ref_axis',(1.,0.,0.));
#7450=DIRECTION('center_axis',(0.,0.,-1.));
#7451=DIRECTION('ref_axis',(1.,0.,0.));
#7452=DIRECTION('',(0.,0.,-1.));
#7453=DIRECTION('center_axis',(0.,0.,1.));
#7454=DIRECTION('ref_axis',(1.,0.,0.));
#7455=DIRECTION('center_axis',(0.,0.,-1.));
#7456=DIRECTION('ref_axis',(1.,0.,0.));
#7457=DIRECTION('center_axis',(0.,0.,-1.));
#7458=DIRECTION('ref_axis',(1.,0.,0.));
#7459=DIRECTION('',(0.,0.,-1.));
#7460=DIRECTION('center_axis',(0.,0.,1.));
#7461=DIRECTION('ref_axis',(1.,0.,0.));
#7462=DIRECTION('center_axis',(1.,0.,0.));
#7463=DIRECTION('ref_axis',(0.,0.,-1.));
#7464=DIRECTION('',(0.,0.,-1.));
#7465=DIRECTION('',(0.,-0.894427190999916,0.447213595499958));
#7466=DIRECTION('',(0.,1.,0.));
#7467=DIRECTION('center_axis',(0.,0.447213595499958,0.894427190999916));
#7468=DIRECTION('ref_axis',(0.,-0.894427190999916,0.447213595499958));
#7469=DIRECTION('',(0.,-0.894427190999916,0.447213595499958));
#7470=DIRECTION('',(-1.,0.,0.));
#7471=DIRECTION('',(-1.,0.,0.));
#7472=DIRECTION('center_axis',(1.,0.,0.));
#7473=DIRECTION('ref_axis',(0.,2.22044604925031E-16,1.));
#7474=DIRECTION('',(0.,0.,1.));
#7475=DIRECTION('',(0.,-1.,0.));
#7476=DIRECTION('center_axis',(0.,-1.,0.));
#7477=DIRECTION('ref_axis',(1.,0.,0.));
#7478=DIRECTION('',(-1.,0.,0.));
#7479=DIRECTION('',(0.,0.,1.));
#7480=DIRECTION('',(-1.,0.,0.));
#7481=DIRECTION('',(0.,0.,-1.));
#7482=DIRECTION('',(1.,0.,0.));
#7483=DIRECTION('',(0.,0.,-1.));
#7484=DIRECTION('center_axis',(1.,0.,0.));
#7485=DIRECTION('ref_axis',(0.,0.,-1.));
#7486=DIRECTION('',(0.,-1.,0.));
#7487=DIRECTION('',(0.,0.707106781186547,0.707106781186548));
#7488=DIRECTION('center_axis',(0.,0.707106781186548,-0.707106781186547));
#7489=DIRECTION('ref_axis',(0.,0.707106781186547,0.707106781186548));
#7490=DIRECTION('',(0.,0.707106781186547,0.707106781186548));
#7491=DIRECTION('',(1.,0.,0.));
#7492=DIRECTION('center_axis',(1.,0.,0.));
#7493=DIRECTION('ref_axis',(0.,2.22044604925031E-16,1.));
#7494=DIRECTION('',(0.,1.,0.));
#7495=DIRECTION('',(0.,0.,1.));
#7496=DIRECTION('center_axis',(0.,0.,1.));
#7497=DIRECTION('ref_axis',(1.,0.,0.));
#7498=DIRECTION('center_axis',(0.,0.,1.));
#7499=DIRECTION('ref_axis',(1.,0.,0.));
#7500=DIRECTION('',(0.865426285481126,-0.501036270541705,0.));
#7501=DIRECTION('',(1.,0.,0.));
#7502=DIRECTION('',(0.,1.,0.));
#7503=DIRECTION('',(-1.,0.,0.));
#7504=DIRECTION('',(-0.707106781186548,0.707106781186548,0.));
#7505=DIRECTION('',(-0.447213595499958,-0.894427190999916,0.));
#7506=DIRECTION('center_axis',(0.,0.,1.));
#7507=DIRECTION('ref_axis',(1.,0.,0.));
#7508=DIRECTION('',(0.,1.,0.));
#7509=DIRECTION('',(-1.,0.,0.));
#7510=DIRECTION('',(-0.961523947640823,-0.274721127897378,0.));
#7511=DIRECTION('',(0.,-1.,0.));
#7512=DIRECTION('',(1.,0.,0.));
#7513=DIRECTION('center_axis',(1.,0.,0.));
#7514=DIRECTION('ref_axis',(0.,1.,0.));
#7515=DIRECTION('',(0.,-1.,0.));
#7516=DIRECTION('',(0.,0.,1.));
#7517=DIRECTION('',(0.,1.,0.));
#7518=DIRECTION('center_axis',(0.,0.,1.));
#7519=DIRECTION('ref_axis',(1.,0.,0.));
#7520=DIRECTION('',(-1.,0.,0.));
#7521=DIRECTION('',(0.,1.,0.));
#7522=DIRECTION('',(0.961523947640823,0.274721127897378,0.));
#7523=DIRECTION('',(1.,0.,0.));
#7524=DIRECTION('center_axis',(0.,-1.,0.));
#7525=DIRECTION('ref_axis',(1.,0.,0.));
#7526=DIRECTION('',(0.,0.,1.));
#7527=DIRECTION('center_axis',(1.,0.,0.));
#7528=DIRECTION('ref_axis',(0.,1.,0.));
#7529=DIRECTION('',(0.,0.,1.));
#7530=DIRECTION('',(0.,-1.,0.));
#7531=DIRECTION('',(0.,0.,1.));
#7532=DIRECTION('center_axis',(-1.,0.,0.));
#7533=DIRECTION('ref_axis',(0.,-1.,0.));
#7534=DIRECTION('',(0.,0.,1.));
#7535=DIRECTION('center_axis',(-0.274721127897378,0.961523947640823,0.));
#7536=DIRECTION('ref_axis',(-0.961523947640823,-0.274721127897378,0.));
#7537=DIRECTION('',(0.,0.,1.));
#7538=DIRECTION('center_axis',(0.,1.,0.));
#7539=DIRECTION('ref_axis',(-1.,0.,0.));
#7540=DIRECTION('',(1.,0.,0.));
#7541=DIRECTION('center_axis',(0.,0.,1.));
#7542=DIRECTION('ref_axis',(1.,0.,0.));
#7543=DIRECTION('center_axis',(0.,0.,1.));
#7544=DIRECTION('ref_axis',(1.,0.,0.));
#7545=DIRECTION('',(-0.447213595499958,-0.894427190999916,0.));
#7546=DIRECTION('',(-0.707106781186548,0.707106781186548,0.));
#7547=DIRECTION('',(-1.,0.,0.));
#7548=DIRECTION('',(0.,1.,0.));
#7549=DIRECTION('',(1.,0.,0.));
#7550=DIRECTION('',(0.865426285481126,-0.501036270541705,0.));
#7551=DIRECTION('center_axis',(0.,0.,1.));
#7552=DIRECTION('ref_axis',(1.,0.,0.));
#7553=DIRECTION('center_axis',(0.,0.,1.));
#7554=DIRECTION('ref_axis',(1.,0.,0.));
#7555=DIRECTION('',(0.,0.,-1.));
#7556=DIRECTION('center_axis',(-0.501036270541705,-0.865426285481126,0.));
#7557=DIRECTION('ref_axis',(0.865426285481126,-0.501036270541705,0.));
#7558=DIRECTION('',(0.,0.,1.));
#7559=DIRECTION('',(0.,0.,1.));
#7560=DIRECTION('center_axis',(-0.894427190999916,0.447213595499958,0.));
#7561=DIRECTION('ref_axis',(-0.447213595499958,-0.894427190999916,0.));
#7562=DIRECTION('',(0.,0.,1.));
#7563=DIRECTION('center_axis',(0.707106781186548,0.707106781186548,0.));
#7564=DIRECTION('ref_axis',(-0.707106781186548,0.707106781186548,0.));
#7565=DIRECTION('',(0.,0.,1.));
#7566=DIRECTION('center_axis',(0.,1.,0.));
#7567=DIRECTION('ref_axis',(-1.,0.,0.));
#7568=DIRECTION('',(0.,0.,1.));
#7569=DIRECTION('center_axis',(1.,0.,0.));
#7570=DIRECTION('ref_axis',(0.,1.,0.));
#7571=DIRECTION('',(0.,0.,1.));
#7572=DIRECTION('center_axis',(0.,-1.,0.));
#7573=DIRECTION('ref_axis',(1.,0.,0.));
#7574=DIRECTION('center_axis',(0.,0.,1.));
#7575=DIRECTION('ref_axis',(1.,0.,0.));
#7576=DIRECTION('axis',(0.,0.,1.));
#7577=DIRECTION('refdir',(1.,0.,0.));
#7578=DIRECTION('center_axis',(0.,0.,-1.));
#7579=DIRECTION('ref_axis',(1.,0.,0.));
#7580=DIRECTION('center_axis',(0.,0.,-1.));
#7581=DIRECTION('ref_axis',(1.,0.,0.));
#7582=DIRECTION('',(0.,0.,-1.));
#7583=DIRECTION('center_axis',(0.,0.,1.));
#7584=DIRECTION('ref_axis',(1.,0.,0.));
#7585=DIRECTION('center_axis',(0.,0.,-1.));
#7586=DIRECTION('ref_axis',(1.,0.,0.));
#7587=DIRECTION('center_axis',(0.,0.,-1.));
#7588=DIRECTION('ref_axis',(1.,0.,0.));
#7589=DIRECTION('',(0.,0.,-1.));
#7590=DIRECTION('center_axis',(0.,0.,1.));
#7591=DIRECTION('ref_axis',(1.,0.,0.));
#7592=DIRECTION('center_axis',(0.,0.,-1.));
#7593=DIRECTION('ref_axis',(1.,0.,0.));
#7594=DIRECTION('center_axis',(0.,0.,-1.));
#7595=DIRECTION('ref_axis',(1.,0.,0.));
#7596=DIRECTION('',(0.,0.,-1.));
#7597=DIRECTION('center_axis',(0.,0.,1.));
#7598=DIRECTION('ref_axis',(1.,0.,0.));
#7599=DIRECTION('center_axis',(1.,0.,0.));
#7600=DIRECTION('ref_axis',(0.,1.,0.));
#7601=DIRECTION('',(0.,-1.,0.));
#7602=DIRECTION('',(0.,0.,1.));
#7603=DIRECTION('',(0.,1.,0.));
#7604=DIRECTION('',(0.,0.,1.));
#7605=DIRECTION('center_axis',(0.,0.,1.));
#7606=DIRECTION('ref_axis',(1.,0.,0.));
#7607=DIRECTION('',(1.,0.,0.));
#7608=DIRECTION('',(-1.,0.,0.));
#7609=DIRECTION('',(0.,1.,0.));
#7610=DIRECTION('',(0.961523947640823,0.274721127897378,0.));
#7611=DIRECTION('center_axis',(0.,-1.,0.));
#7612=DIRECTION('ref_axis',(1.,0.,0.));
#7613=DIRECTION('',(0.,0.,-1.));
#7614=DIRECTION('',(1.,0.,0.));
#7615=DIRECTION('',(0.,0.,1.));
#7616=DIRECTION('',(-1.,0.,0.));
#7617=DIRECTION('center_axis',(1.,0.,0.));
#7618=DIRECTION('ref_axis',(0.,1.,0.));
#7619=DIRECTION('',(0.,0.,1.));
#7620=DIRECTION('',(0.,-1.,0.));
#7621=DIRECTION('',(0.,0.,1.));
#7622=DIRECTION('',(0.,1.,0.));
#7623=DIRECTION('center_axis',(-1.,0.,0.));
#7624=DIRECTION('ref_axis',(0.,-1.,0.));
#7625=DIRECTION('',(0.,-1.,0.));
#7626=DIRECTION('',(0.,0.,1.));
#7627=DIRECTION('center_axis',(-0.274721127897378,0.961523947640823,0.));
#7628=DIRECTION('ref_axis',(-0.961523947640823,-0.274721127897378,0.));
#7629=DIRECTION('',(-0.961523947640823,-0.274721127897378,0.));
#7630=DIRECTION('',(0.,0.,1.));
#7631=DIRECTION('center_axis',(0.,1.,0.));
#7632=DIRECTION('ref_axis',(-1.,0.,0.));
#7633=DIRECTION('',(-1.,0.,0.));
#7634=DIRECTION('',(1.,0.,0.));
#7635=DIRECTION('center_axis',(0.,0.,1.));
#7636=DIRECTION('ref_axis',(1.,0.,0.));
#7637=DIRECTION('center_axis',(0.,0.,1.));
#7638=DIRECTION('ref_axis',(1.,0.,0.));
#7639=DIRECTION('',(-0.447213595499958,-0.894427190999916,0.));
#7640=DIRECTION('',(-0.707106781186548,0.707106781186548,0.));
#7641=DIRECTION('',(-1.,0.,0.));
#7642=DIRECTION('',(0.,1.,0.));
#7643=DIRECTION('',(1.,0.,0.));
#7644=DIRECTION('',(0.865426285481126,-0.501036270541705,0.));
#7645=DIRECTION('center_axis',(0.,0.,1.));
#7646=DIRECTION('ref_axis',(1.,0.,0.));
#7647=DIRECTION('center_axis',(0.,0.,1.));
#7648=DIRECTION('ref_axis',(1.,0.,0.));
#7649=DIRECTION('center_axis',(0.,0.,1.));
#7650=DIRECTION('ref_axis',(1.,0.,0.));
#7651=DIRECTION('',(0.,0.,-1.));
#7652=DIRECTION('center_axis',(-0.501036270541705,-0.865426285481126,0.));
#7653=DIRECTION('ref_axis',(0.865426285481126,-0.501036270541705,0.));
#7654=DIRECTION('',(0.,0.,1.));
#7655=DIRECTION('',(0.,0.,1.));
#7656=DIRECTION('',(0.865426285481126,-0.501036270541705,0.));
#7657=DIRECTION('center_axis',(-0.894427190999916,0.447213595499958,0.));
#7658=DIRECTION('ref_axis',(-0.447213595499958,-0.894427190999916,0.));
#7659=DIRECTION('',(-0.447213595499958,-0.894427190999916,0.));
#7660=DIRECTION('',(0.,0.,1.));
#7661=DIRECTION('center_axis',(0.707106781186548,0.707106781186548,0.));
#7662=DIRECTION('ref_axis',(-0.707106781186548,0.707106781186548,0.));
#7663=DIRECTION('',(-0.707106781186548,0.707106781186548,0.));
#7664=DIRECTION('',(0.,0.,1.));
#7665=DIRECTION('center_axis',(0.,1.,0.));
#7666=DIRECTION('ref_axis',(-1.,0.,0.));
#7667=DIRECTION('',(-1.,0.,0.));
#7668=DIRECTION('',(0.,0.,1.));
#7669=DIRECTION('center_axis',(1.,0.,0.));
#7670=DIRECTION('ref_axis',(0.,1.,0.));
#7671=DIRECTION('',(0.,1.,0.));
#7672=DIRECTION('',(0.,0.,1.));
#7673=DIRECTION('center_axis',(0.,-1.,0.));
#7674=DIRECTION('ref_axis',(1.,0.,0.));
#7675=DIRECTION('',(1.,0.,0.));
#7676=DIRECTION('center_axis',(0.,0.,1.));
#7677=DIRECTION('ref_axis',(1.,0.,0.));
#7678=DIRECTION('center_axis',(0.,0.,1.));
#7679=DIRECTION('ref_axis',(1.,0.,0.));
#7680=DIRECTION('center_axis',(0.,0.,1.));
#7681=DIRECTION('ref_axis',(1.,0.,0.));
#7682=DIRECTION('axis',(0.,0.,1.));
#7683=DIRECTION('refdir',(1.,0.,0.));
#7684=DIRECTION('center_axis',(0.,0.,1.));
#7685=DIRECTION('ref_axis',(1.,0.,0.));
#7686=DIRECTION('center_axis',(0.,0.,1.));
#7687=DIRECTION('ref_axis',(1.,0.,0.));
#7688=DIRECTION('',(0.,0.,1.));
#7689=DIRECTION('center_axis',(0.,0.,1.));
#7690=DIRECTION('ref_axis',(1.,0.,0.));
#7691=DIRECTION('center_axis',(0.,0.,-1.));
#7692=DIRECTION('ref_axis',(-1.,0.,0.));
#7693=DIRECTION('center_axis',(0.,0.,-1.));
#7694=DIRECTION('ref_axis',(1.,0.,0.));
#7695=DIRECTION('center_axis',(0.,0.,1.));
#7696=DIRECTION('ref_axis',(1.,0.,0.));
#7697=DIRECTION('center_axis',(0.,0.,1.));
#7698=DIRECTION('ref_axis',(1.,0.,0.));
#7699=DIRECTION('center_axis',(0.,0.,1.));
#7700=DIRECTION('ref_axis',(1.,0.,0.));
#7701=DIRECTION('center_axis',(0.,0.,1.));
#7702=DIRECTION('ref_axis',(1.,0.,0.));
#7703=DIRECTION('',(0.,0.,-1.));
#7704=DIRECTION('center_axis',(0.,0.,1.));
#7705=DIRECTION('ref_axis',(1.,0.,0.));
#7706=DIRECTION('center_axis',(0.,0.,1.));
#7707=DIRECTION('ref_axis',(1.,0.,0.));
#7708=DIRECTION('center_axis',(0.,0.,1.));
#7709=DIRECTION('ref_axis',(1.,0.,0.));
#7710=DIRECTION('center_axis',(0.,0.,1.));
#7711=DIRECTION('ref_axis',(1.,0.,0.));
#7712=DIRECTION('',(0.,0.,-1.));
#7713=DIRECTION('center_axis',(0.,0.,1.));
#7714=DIRECTION('ref_axis',(1.,0.,0.));
#7715=DIRECTION('center_axis',(0.,0.,1.));
#7716=DIRECTION('ref_axis',(1.,0.,0.));
#7717=DIRECTION('center_axis',(0.,0.,1.));
#7718=DIRECTION('ref_axis',(1.,0.,0.));
#7719=DIRECTION('',(0.,0.,-1.));
#7720=DIRECTION('center_axis',(0.,0.,1.));
#7721=DIRECTION('ref_axis',(1.,0.,0.));
#7722=DIRECTION('axis',(0.,0.,1.));
#7723=DIRECTION('refdir',(1.,0.,0.));
#7724=DIRECTION('center_axis',(-1.,0.,0.));
#7725=DIRECTION('ref_axis',(0.,1.,0.));
#7726=DIRECTION('',(0.,0.,1.));
#7727=DIRECTION('',(0.,-1.,0.));
#7728=DIRECTION('',(0.,0.,-1.));
#7729=DIRECTION('',(0.,1.,0.));
#7730=DIRECTION('center_axis',(1.,0.,0.));
#7731=DIRECTION('ref_axis',(0.,-1.,0.));
#7732=DIRECTION('',(0.,0.,-1.));
#7733=DIRECTION('',(0.,-1.,0.));
#7734=DIRECTION('',(0.,0.,1.));
#7735=DIRECTION('',(0.,1.,0.));
#7736=DIRECTION('center_axis',(0.,0.,1.));
#7737=DIRECTION('ref_axis',(1.,0.,0.));
#7738=DIRECTION('center_axis',(0.,0.,1.));
#7739=DIRECTION('ref_axis',(1.,0.,0.));
#7740=DIRECTION('center_axis',(0.,0.,-1.));
#7741=DIRECTION('ref_axis',(1.,0.,0.));
#7742=DIRECTION('center_axis',(0.,0.,1.));
#7743=DIRECTION('ref_axis',(6.12323399573677E-17,-1.,0.));
#7744=DIRECTION('center_axis',(0.,0.,-1.));
#7745=DIRECTION('ref_axis',(1.,0.,0.));
#7746=DIRECTION('center_axis',(0.,0.,1.));
#7747=DIRECTION('ref_axis',(6.12323399573677E-17,-1.,0.));
#7748=DIRECTION('center_axis',(0.,0.,1.));
#7749=DIRECTION('ref_axis',(1.,0.,0.));
#7750=DIRECTION('center_axis',(0.,0.,1.));
#7751=DIRECTION('ref_axis',(1.,0.,0.));
#7752=DIRECTION('axis',(0.,0.,1.));
#7753=DIRECTION('refdir',(1.,0.,0.));
#7754=DIRECTION('axis',(0.,0.,1.));
#7755=DIRECTION('refdir',(1.,0.,0.));
#7756=DIRECTION('center_axis',(-9.61618982193066E-33,1.03600583455278E-18,
1.));
#7757=DIRECTION('ref_axis',(1.,0.,9.61618982193066E-33));
#7758=DIRECTION('',(0.,-1.,1.03600583455278E-18));
#7759=DIRECTION('',(0.,1.,-1.03600583455278E-18));
#7760=DIRECTION('center_axis',(-9.61618982193066E-33,1.03600583455278E-18,
1.));
#7761=DIRECTION('ref_axis',(1.,0.,0.));
#7762=DIRECTION('center_axis',(-9.61618982193066E-33,1.03600583455278E-18,
1.));
#7763=DIRECTION('ref_axis',(1.,0.,0.));
#7764=DIRECTION('center_axis',(-9.61618982193066E-33,1.03600583455278E-18,
1.));
#7765=DIRECTION('ref_axis',(1.,0.,0.));
#7766=DIRECTION('center_axis',(0.,0.,-1.));
#7767=DIRECTION('ref_axis',(1.,0.,0.));
#7768=DIRECTION('center_axis',(9.61618982193066E-33,-1.03600583455278E-18,
-1.));
#7769=DIRECTION('ref_axis',(1.,0.,0.));
#7770=DIRECTION('',(0.,0.,-1.));
#7771=DIRECTION('center_axis',(-9.61618982193066E-33,1.03600583455278E-18,
1.));
#7772=DIRECTION('ref_axis',(1.,0.,0.));
#7773=DIRECTION('center_axis',(0.,0.,-1.));
#7774=DIRECTION('ref_axis',(1.,0.,0.));
#7775=DIRECTION('center_axis',(9.61618982193066E-33,-1.03600583455278E-18,
-1.));
#7776=DIRECTION('ref_axis',(1.,0.,0.));
#7777=DIRECTION('',(0.,0.,-1.));
#7778=DIRECTION('center_axis',(0.,0.,-1.));
#7779=DIRECTION('ref_axis',(1.,0.,0.));
#7780=DIRECTION('center_axis',(9.61618982193066E-33,-1.03600583455278E-18,
-1.));
#7781=DIRECTION('ref_axis',(1.,0.,0.));
#7782=DIRECTION('',(0.,0.,-1.));
#7783=DIRECTION('center_axis',(0.,0.,-1.));
#7784=DIRECTION('ref_axis',(1.,0.,0.));
#7785=DIRECTION('center_axis',(9.61618982193066E-33,-1.03600583455278E-18,
-1.));
#7786=DIRECTION('ref_axis',(1.,0.,0.));
#7787=DIRECTION('',(0.,0.,-1.));
#7788=DIRECTION('center_axis',(-9.61618982193066E-33,1.03600583455278E-18,
1.));
#7789=DIRECTION('ref_axis',(1.,0.,0.));
#7790=DIRECTION('center_axis',(0.,0.,-1.));
#7791=DIRECTION('ref_axis',(1.,0.,0.));
#7792=DIRECTION('center_axis',(9.61618982193066E-33,-1.03600583455278E-18,
-1.));
#7793=DIRECTION('ref_axis',(1.,0.,0.));
#7794=DIRECTION('',(0.,0.,-1.));
#7795=DIRECTION('center_axis',(0.,0.,-1.));
#7796=DIRECTION('ref_axis',(1.,0.,0.));
#7797=DIRECTION('center_axis',(0.,0.,-1.));
#7798=DIRECTION('ref_axis',(1.,0.,0.));
#7799=DIRECTION('center_axis',(0.,0.,1.));
#7800=DIRECTION('ref_axis',(1.,0.,0.));
#7801=DIRECTION('center_axis',(0.,0.,-1.));
#7802=DIRECTION('ref_axis',(1.,0.,0.));
#7803=DIRECTION('center_axis',(9.61618982193066E-33,-1.03600583455278E-18,
-1.));
#7804=DIRECTION('ref_axis',(1.,0.,0.));
#7805=DIRECTION('',(0.,0.,-1.));
#7806=DIRECTION('center_axis',(0.,0.,-1.));
#7807=DIRECTION('ref_axis',(1.,0.,0.));
#7808=DIRECTION('center_axis',(0.,0.,-1.));
#7809=DIRECTION('ref_axis',(1.,0.,0.));
#7810=DIRECTION('center_axis',(0.,0.,1.));
#7811=DIRECTION('ref_axis',(1.,0.,0.));
#7812=DIRECTION('center_axis',(0.,0.,-1.));
#7813=DIRECTION('ref_axis',(1.,0.,0.));
#7814=DIRECTION('',(0.,0.,-1.));
#7815=DIRECTION('center_axis',(0.,0.,1.));
#7816=DIRECTION('ref_axis',(1.,0.,0.));
#7817=DIRECTION('center_axis',(0.,0.,-1.));
#7818=DIRECTION('ref_axis',(1.,0.,0.));
#7819=DIRECTION('',(0.,0.,-1.));
#7820=DIRECTION('center_axis',(0.,0.,1.));
#7821=DIRECTION('ref_axis',(1.,0.,0.));
#7822=DIRECTION('center_axis',(0.,-1.,0.));
#7823=DIRECTION('ref_axis',(-1.,0.,0.));
#7824=DIRECTION('',(0.0523359562429438,0.,0.998629534754574));
#7825=DIRECTION('',(1.,0.,0.));
#7826=DIRECTION('',(-0.0523359562429438,0.,-0.998629534754574));
#7827=DIRECTION('',(1.,0.,0.));
#7828=DIRECTION('center_axis',(0.,-1.,0.));
#7829=DIRECTION('ref_axis',(-1.,0.,0.));
#7830=DIRECTION('',(0.,0.,-1.));
#7831=DIRECTION('',(1.,0.,0.));
#7832=DIRECTION('',(0.,0.,1.));
#7833=DIRECTION('',(1.,0.,0.));
#7834=DIRECTION('center_axis',(0.,-1.,0.));
#7835=DIRECTION('ref_axis',(-1.,0.,0.));
#7836=DIRECTION('',(0.,0.,-1.));
#7837=DIRECTION('',(1.,0.,0.));
#7838=DIRECTION('',(0.,0.,1.));
#7839=DIRECTION('',(1.,0.,0.));
#7840=DIRECTION('center_axis',(0.,-1.,0.));
#7841=DIRECTION('ref_axis',(-1.,0.,0.));
#7842=DIRECTION('',(0.,0.,-1.));
#7843=DIRECTION('',(1.,0.,0.));
#7844=DIRECTION('',(0.,0.,1.));
#7845=DIRECTION('',(1.,0.,0.));
#7846=DIRECTION('center_axis',(0.,1.,0.));
#7847=DIRECTION('ref_axis',(1.,0.,0.));
#7848=DIRECTION('',(-0.0523359562429438,0.,-0.998629534754574));
#7849=DIRECTION('',(-1.,0.,0.));
#7850=DIRECTION('',(0.0523359562429438,0.,0.998629534754574));
#7851=DIRECTION('',(-1.,0.,0.));
#7852=DIRECTION('center_axis',(0.,1.,0.));
#7853=DIRECTION('ref_axis',(1.,0.,0.));
#7854=DIRECTION('',(0.,0.,1.));
#7855=DIRECTION('',(-1.,0.,0.));
#7856=DIRECTION('',(0.,0.,-1.));
#7857=DIRECTION('',(-1.,0.,0.));
#7858=DIRECTION('center_axis',(0.,1.,0.));
#7859=DIRECTION('ref_axis',(1.,0.,0.));
#7860=DIRECTION('',(0.,0.,1.));
#7861=DIRECTION('',(-1.,0.,0.));
#7862=DIRECTION('',(0.,0.,-1.));
#7863=DIRECTION('',(-1.,0.,0.));
#7864=DIRECTION('center_axis',(0.,0.,1.));
#7865=DIRECTION('ref_axis',(1.,0.,0.));
#7866=DIRECTION('center_axis',(0.,0.,1.));
#7867=DIRECTION('ref_axis',(1.,0.,0.));
#7868=DIRECTION('center_axis',(0.,0.,1.));
#7869=DIRECTION('ref_axis',(1.,0.,0.));
#7870=DIRECTION('center_axis',(0.,0.,1.));
#7871=DIRECTION('ref_axis',(1.,0.,0.));
#7872=DIRECTION('center_axis',(0.,0.,1.));
#7873=DIRECTION('ref_axis',(1.,0.,0.));
#7874=DIRECTION('',(0.,1.,0.));
#7875=DIRECTION('',(0.,-1.,0.));
#7876=DIRECTION('center_axis',(0.,0.,1.));
#7877=DIRECTION('ref_axis',(1.,0.,0.));
#7878=DIRECTION('',(0.,-1.,0.));
#7879=DIRECTION('',(0.,1.,0.));
#7880=DIRECTION('center_axis',(0.,0.,1.));
#7881=DIRECTION('ref_axis',(1.,0.,0.));
#7882=DIRECTION('',(0.,-1.,0.));
#7883=DIRECTION('',(0.,1.,0.));
#7884=DIRECTION('center_axis',(0.,0.,1.));
#7885=DIRECTION('ref_axis',(1.,0.,0.));
#7886=DIRECTION('',(0.,-1.,0.));
#7887=DIRECTION('',(-1.,0.,0.));
#7888=DIRECTION('',(0.,1.,0.));
#7889=DIRECTION('center_axis',(0.,1.,0.));
#7890=DIRECTION('ref_axis',(1.,0.,0.));
#7891=DIRECTION('',(0.,0.,1.));
#7892=DIRECTION('',(-1.,0.,0.));
#7893=DIRECTION('',(0.,0.,-1.));
#7894=DIRECTION('center_axis',(-1.,0.,0.));
#7895=DIRECTION('ref_axis',(0.,-1.,0.));
#7896=DIRECTION('',(0.,-1.,0.));
#7897=DIRECTION('',(0.,-1.,1.03600583455278E-18));
#7898=DIRECTION('center_axis',(1.,0.,0.));
#7899=DIRECTION('ref_axis',(0.,1.,0.));
#7900=DIRECTION('',(0.,1.,0.));
#7901=DIRECTION('',(0.,1.,-1.03600583455278E-18));
#7902=DIRECTION('',(0.,1.,0.));
#7903=DIRECTION('center_axis',(1.,0.,0.));
#7904=DIRECTION('ref_axis',(0.,1.,0.));
#7905=DIRECTION('',(0.,1.,0.));
#7906=DIRECTION('',(0.,1.,-1.03600583455278E-18));
#7907=DIRECTION('',(0.,1.,0.));
#7908=DIRECTION('center_axis',(1.,0.,0.));
#7909=DIRECTION('ref_axis',(0.,1.,0.));
#7910=DIRECTION('',(0.,1.,0.));
#7911=DIRECTION('',(0.,1.,0.));
#7912=DIRECTION('center_axis',(0.998629534754574,0.,-0.0523359562429438));
#7913=DIRECTION('ref_axis',(-0.0523359562429438,0.,-0.998629534754574));
#7914=DIRECTION('',(0.,-1.,0.));
#7915=DIRECTION('',(5.42947651131849E-20,-1.,1.03600583455278E-18));
#7916=DIRECTION('',(0.,-1.,0.));
#7917=DIRECTION('center_axis',(0.,0.,1.));
#7918=DIRECTION('ref_axis',(1.,0.,0.));
#7919=DIRECTION('',(0.,-1.,0.));
#7920=DIRECTION('',(0.,-1.,0.));
#7921=DIRECTION('',(0.,-1.,0.));
#7922=DIRECTION('',(0.,1.,0.));
#7923=DIRECTION('',(0.,-1.,0.));
#7924=DIRECTION('',(0.,1.,0.));
#7925=DIRECTION('',(0.,-1.,0.));
#7926=DIRECTION('',(0.,-1.,0.));
#7927=DIRECTION('',(0.,-1.,0.));
#7928=DIRECTION('',(0.,1.,0.));
#7929=DIRECTION('',(0.,1.,0.));
#7930=DIRECTION('center_axis',(0.,0.,1.));
#7931=DIRECTION('ref_axis',(1.,0.,0.));
#7932=DIRECTION('center_axis',(-9.61618982193066E-33,1.03600583455278E-18,
1.));
#7933=DIRECTION('ref_axis',(1.,0.,0.));
#7934=DIRECTION('',(0.,0.,-1.));
#7935=DIRECTION('center_axis',(0.,0.,1.));
#7936=DIRECTION('ref_axis',(1.,0.,0.));
#7937=DIRECTION('',(0.,0.,-1.));
#7938=DIRECTION('center_axis',(1.,0.,0.));
#7939=DIRECTION('ref_axis',(0.,1.,0.));
#7940=DIRECTION('',(0.,1.,-1.03600583455278E-18));
#7941=DIRECTION('center_axis',(0.994044372876412,-0.108976074221552,-1.1933167131821E-14));
#7942=DIRECTION('ref_axis',(-0.108857570442347,-0.992963419871597,0.0466226999892957));
#7943=DIRECTION('center_axis',(-9.61618982193066E-33,1.03600583455278E-18,
1.));
#7944=DIRECTION('ref_axis',(1.,0.,9.61618982193066E-33));
#7945=DIRECTION('center_axis',(-9.61618982193066E-33,1.03600583455278E-18,
1.));
#7946=DIRECTION('ref_axis',(1.,0.,9.61618982193066E-33));
#7947=DIRECTION('',(-5.42947651131849E-20,-1.,1.03600583455278E-18));
#7948=DIRECTION('center_axis',(-1.,0.,0.));
#7949=DIRECTION('ref_axis',(0.,-1.,0.));
#7950=DIRECTION('',(0.,-1.,1.03600583455278E-18));
#7951=DIRECTION('center_axis',(-9.61618982193066E-33,1.03600583455278E-18,
1.));
#7952=DIRECTION('ref_axis',(1.,0.,9.61618982193066E-33));
#7953=DIRECTION('center_axis',(-1.,0.,0.));
#7954=DIRECTION('ref_axis',(0.,-1.,0.));
#7955=DIRECTION('center_axis',(-1.,0.,0.));
#7956=DIRECTION('ref_axis',(0.,-1.,0.));
#7957=DIRECTION('',(0.,-1.,1.03600583455278E-18));
#7958=DIRECTION('center_axis',(-0.999738255753194,0.0228783737088345,0.));
#7959=DIRECTION('ref_axis',(0.,0.,1.));
#7960=DIRECTION('center_axis',(-9.61618982193066E-33,1.03600583455278E-18,
1.));
#7961=DIRECTION('ref_axis',(1.,0.,9.61618982193066E-33));
#7962=DIRECTION('',(-5.42947651131849E-20,1.,-1.03600583455278E-18));
#7963=DIRECTION('center_axis',(-0.999738255790058,-0.0228783720979604,1.69987959829136E-9));
#7964=DIRECTION('ref_axis',(-0.022845652001536,0.998308458201847,0.0534630570326489));
#7965=DIRECTION('center_axis',(-0.375013085256251,-0.833398400631247,0.405970801550885));
#7966=DIRECTION('ref_axis',(-0.565498005067694,0.552672693214782,0.612180447612612));
#7967=DIRECTION('center_axis',(-7.78474640228738E-11,1.,0.));
#7968=DIRECTION('ref_axis',(0.,0.,1.));
#7969=DIRECTION('center_axis',(0.0522645732252412,-0.0522112666801462,0.997267465636596));
#7970=DIRECTION('ref_axis',(-0.998629534754574,0.,0.0523359562429445));
#7971=DIRECTION('center_axis',(0.361627795167438,-0.818371417997736,0.44664701943113));
#7972=DIRECTION('ref_axis',(0.514966362801186,0.574689674697898,0.636035708886648));
#7973=DIRECTION('center_axis',(0.994044372876412,0.108976074221546,-5.96658356591051E-15));
#7974=DIRECTION('ref_axis',(5.9211894646675E-15,7.40148683083438E-16,1.));
#7975=DIRECTION('center_axis',(-0.052263633556273,-0.0525535553916586,0.997249535684621));
#7976=DIRECTION('ref_axis',(-0.108857570442347,0.992963419871597,0.0466226999892949));
#7977=DIRECTION('center_axis',(0.,1.,0.));
#7978=DIRECTION('ref_axis',(0.998629534754574,0.,0.0523359562429438));
#7979=DIRECTION('center_axis',(0.375013085403515,-0.833398400816333,-0.405970801034895));
#7980=DIRECTION('ref_axis',(-0.565498005700927,-0.552672692935682,0.612180447279637));
#7981=DIRECTION('center_axis',(0.0522645732252408,0.0522112666801459,0.997267465636596));
#7982=DIRECTION('ref_axis',(-0.0228456520015352,-0.998308458201847,0.0534630570326489));
#7983=DIRECTION('center_axis',(-4.07418268117644E-12,-1.,-7.77400366303027E-11));
#7984=DIRECTION('ref_axis',(-0.998629534754574,0.,0.0523359562429438));
#7985=DIRECTION('center_axis',(-5.42947651131849E-20,1.,-1.03600583455278E-18));
#7986=DIRECTION('ref_axis',(-0.688354575693754,0.,0.725374371012288));
#7987=DIRECTION('center_axis',(-0.361627795167436,-0.818371417997736,-0.446647019431131));
#7988=DIRECTION('ref_axis',(0.514966362801185,-0.574689674697896,0.636035708886651));
#7989=DIRECTION('center_axis',(-0.0522636335562752,0.0525535553916633,0.99724953568462));
#7990=DIRECTION('ref_axis',(0.998629534754574,0.,0.0523359562429442));
#7991=DIRECTION('center_axis',(0.,-1.,0.));
#7992=DIRECTION('ref_axis',(0.,0.,1.));
#7993=DIRECTION('center_axis',(-5.42947651131849E-20,-1.,1.03600583455278E-18));
#7994=DIRECTION('ref_axis',(0.688354575693754,0.,0.725374371012288));
#7995=DIRECTION('',(5.42947651131849E-20,1.,-1.03600583455278E-18));
#7996=DIRECTION('center_axis',(-0.998629534754574,0.,-0.0523359562429438));
#7997=DIRECTION('ref_axis',(-0.0523359562429438,0.,0.998629534754574));
#7998=DIRECTION('center_axis',(-0.375013085256251,-0.833398400631247,0.405970801550885));
#7999=DIRECTION('ref_axis',(-0.565498005067695,0.552672693214781,0.612180447612612));
#8000=DIRECTION('center_axis',(-7.78474640228738E-11,1.,0.));
#8001=DIRECTION('ref_axis',(0.,0.,1.));
#8002=DIRECTION('center_axis',(-0.999738255790058,-0.0228783720979604,1.69987959829136E-9));
#8003=DIRECTION('ref_axis',(-0.022845652001536,0.998308458201847,0.0534630570326489));
#8004=DIRECTION('center_axis',(0.0522645732252412,-0.0522112666801462,0.997267465636596));
#8005=DIRECTION('ref_axis',(-0.998629534754574,0.,0.0523359562429445));
#8006=DIRECTION('center_axis',(0.361627795167442,-0.818371417997735,0.446647019431129));
#8007=DIRECTION('ref_axis',(0.514966362801186,0.574689674697898,0.636035708886649));
#8008=DIRECTION('center_axis',(0.994044372876412,0.108976074221546,-5.96658356591051E-15));
#8009=DIRECTION('ref_axis',(5.9211894646675E-15,7.40148683083438E-16,1.));
#8010=DIRECTION('center_axis',(0.,1.,0.));
#8011=DIRECTION('ref_axis',(0.998629534754574,0.,0.0523359562429438));
#8012=DIRECTION('center_axis',(-0.052263633556273,-0.0525535553916586,0.997249535684621));
#8013=DIRECTION('ref_axis',(-0.108857570442347,0.992963419871597,0.0466226999892949));
#8014=DIRECTION('center_axis',(0.375013085403515,-0.833398400816333,-0.405970801034895));
#8015=DIRECTION('ref_axis',(-0.565498005700926,-0.552672692935682,0.612180447279637));
#8016=DIRECTION('center_axis',(-0.999738255753194,0.0228783737088345,0.));
#8017=DIRECTION('ref_axis',(0.,0.,1.));
#8018=DIRECTION('center_axis',(-4.07418268117644E-12,-1.,-7.77400366303027E-11));
#8019=DIRECTION('ref_axis',(-0.998629534754574,0.,0.0523359562429438));
#8020=DIRECTION('center_axis',(0.0522645732252408,0.0522112666801459,0.997267465636596));
#8021=DIRECTION('ref_axis',(-0.0228456520015352,-0.998308458201847,0.0534630570326489));
#8022=DIRECTION('center_axis',(-5.42947651131849E-20,1.,-1.03600583455278E-18));
#8023=DIRECTION('ref_axis',(-0.688354575693754,0.,0.725374371012288));
#8024=DIRECTION('',(5.42947651131849E-20,-1.,1.03600583455278E-18));
#8025=DIRECTION('',(-5.42947651131849E-20,1.,-1.03600583455278E-18));
#8026=DIRECTION('center_axis',(-0.361627795167436,-0.818371417997736,-0.446647019431131));
#8027=DIRECTION('ref_axis',(0.51496636280118,-0.574689674697898,0.636035708886653));
#8028=DIRECTION('center_axis',(-0.0522636335562752,0.0525535553916633,0.99724953568462));
#8029=DIRECTION('ref_axis',(0.998629534754574,0.,0.0523359562429441));
#8030=DIRECTION('center_axis',(0.,-1.,0.));
#8031=DIRECTION('ref_axis',(0.,0.,1.));
#8032=DIRECTION('center_axis',(0.994044372876412,-0.108976074221552,-1.1933167131821E-14));
#8033=DIRECTION('ref_axis',(-0.108857570442347,-0.992963419871597,0.0466226999892957));
#8034=DIRECTION('center_axis',(-5.42947651131849E-20,-1.,1.03600583455278E-18));
#8035=DIRECTION('ref_axis',(0.688354575693754,0.,0.725374371012288));
#8036=DIRECTION('',(5.42947651131849E-20,1.,-1.03600583455278E-18));
#8037=DIRECTION('',(-5.42947651131849E-20,-1.,1.03600583455278E-18));
#8038=DIRECTION('center_axis',(0.998629534754574,0.,-0.0523359562429438));
#8039=DIRECTION('ref_axis',(-0.0523359562429438,0.,-0.998629534754574));
#8040=DIRECTION('center_axis',(-9.61618982193066E-33,1.03600583455278E-18,
1.));
#8041=DIRECTION('ref_axis',(1.,0.,9.61618982193066E-33));
#8042=DIRECTION('center_axis',(-0.998629534754574,0.,-0.0523359562429438));
#8043=DIRECTION('ref_axis',(-0.0523359562429438,0.,0.998629534754574));
#8044=DIRECTION('axis',(0.,0.,1.));
#8045=DIRECTION('refdir',(1.,0.,0.));
#8046=DIRECTION('center_axis',(-9.61618982193066E-33,1.03600583455278E-18,
1.));
#8047=DIRECTION('ref_axis',(1.,0.,9.61618982193066E-33));
#8048=DIRECTION('',(0.,-1.,1.03600583455278E-18));
#8049=DIRECTION('',(0.,1.,-1.03600583455278E-18));
#8050=DIRECTION('center_axis',(-9.61618982193066E-33,1.03600583455278E-18,
1.));
#8051=DIRECTION('ref_axis',(1.,0.,0.));
#8052=DIRECTION('center_axis',(-9.61618982193066E-33,1.03600583455278E-18,
1.));
#8053=DIRECTION('ref_axis',(1.,0.,0.));
#8054=DIRECTION('center_axis',(-9.61618982193066E-33,1.03600583455278E-18,
1.));
#8055=DIRECTION('ref_axis',(1.,0.,0.));
#8056=DIRECTION('center_axis',(0.,0.,-1.));
#8057=DIRECTION('ref_axis',(1.,0.,0.));
#8058=DIRECTION('center_axis',(9.61618982193066E-33,-1.03600583455278E-18,
-1.));
#8059=DIRECTION('ref_axis',(1.,0.,0.));
#8060=DIRECTION('',(0.,0.,-1.));
#8061=DIRECTION('center_axis',(-9.61618982193066E-33,1.03600583455278E-18,
1.));
#8062=DIRECTION('ref_axis',(1.,0.,0.));
#8063=DIRECTION('center_axis',(0.,0.,-1.));
#8064=DIRECTION('ref_axis',(1.,0.,0.));
#8065=DIRECTION('center_axis',(9.61618982193066E-33,-1.03600583455278E-18,
-1.));
#8066=DIRECTION('ref_axis',(1.,0.,0.));
#8067=DIRECTION('',(0.,0.,-1.));
#8068=DIRECTION('center_axis',(0.,0.,-1.));
#8069=DIRECTION('ref_axis',(1.,0.,0.));
#8070=DIRECTION('center_axis',(9.61618982193066E-33,-1.03600583455278E-18,
-1.));
#8071=DIRECTION('ref_axis',(1.,0.,0.));
#8072=DIRECTION('',(0.,0.,-1.));
#8073=DIRECTION('center_axis',(0.,0.,-1.));
#8074=DIRECTION('ref_axis',(1.,0.,0.));
#8075=DIRECTION('center_axis',(9.61618982193066E-33,-1.03600583455278E-18,
-1.));
#8076=DIRECTION('ref_axis',(1.,0.,0.));
#8077=DIRECTION('',(0.,0.,-1.));
#8078=DIRECTION('center_axis',(-9.61618982193066E-33,1.03600583455278E-18,
1.));
#8079=DIRECTION('ref_axis',(1.,0.,0.));
#8080=DIRECTION('center_axis',(0.86602540378444,0.499999999999998,0.));
#8081=DIRECTION('ref_axis',(0.499999999999998,-0.86602540378444,0.));
#8082=DIRECTION('',(0.499999999999998,-0.86602540378444,8.9720737119161E-19));
#8083=DIRECTION('',(0.,0.,-1.));
#8084=DIRECTION('',(0.499999999999998,-0.86602540378444,0.));
#8085=DIRECTION('',(0.,0.,-1.));
#8086=DIRECTION('center_axis',(1.60246890531964E-16,1.,0.));
#8087=DIRECTION('ref_axis',(1.,-1.60246890531964E-16,0.));
#8088=DIRECTION('',(1.,-1.60246890531964E-16,9.78220653549071E-33));
#8089=DIRECTION('',(0.,0.,-1.));
#8090=DIRECTION('',(1.,-1.60246890531964E-16,0.));
#8091=DIRECTION('center_axis',(-0.86602540378444,0.499999999999998,0.));
#8092=DIRECTION('ref_axis',(0.499999999999998,0.86602540378444,0.));
#8093=DIRECTION('',(0.499999999999998,0.86602540378444,-8.97207371191601E-19));
#8094=DIRECTION('',(0.,0.,-1.));
#8095=DIRECTION('',(0.499999999999998,0.86602540378444,0.));
#8096=DIRECTION('center_axis',(-0.86602540378444,-0.499999999999998,0.));
#8097=DIRECTION('ref_axis',(-0.499999999999998,0.86602540378444,0.));
#8098=DIRECTION('',(-0.499999999999998,0.86602540378444,-8.9720737119161E-19));
#8099=DIRECTION('',(0.,0.,-1.));
#8100=DIRECTION('',(-0.499999999999998,0.86602540378444,0.));
#8101=DIRECTION('center_axis',(-1.60246890531964E-16,-1.,0.));
#8102=DIRECTION('ref_axis',(-1.,1.60246890531964E-16,0.));
#8103=DIRECTION('',(-1.,1.60246890531964E-16,-9.78220653549071E-33));
#8104=DIRECTION('',(0.,0.,-1.));
#8105=DIRECTION('',(-1.,1.60246890531964E-16,0.));
#8106=DIRECTION('center_axis',(0.86602540378444,-0.499999999999998,0.));
#8107=DIRECTION('ref_axis',(-0.499999999999998,-0.86602540378444,0.));
#8108=DIRECTION('',(-0.499999999999998,-0.86602540378444,8.97207371191601E-19));
#8109=DIRECTION('',(-0.499999999999998,-0.86602540378444,0.));
#8110=DIRECTION('center_axis',(0.,0.,-1.));
#8111=DIRECTION('ref_axis',(-1.,0.,0.));
#8112=DIRECTION('center_axis',(0.,0.,1.));
#8113=DIRECTION('ref_axis',(1.,0.,0.));
#8114=DIRECTION('center_axis',(0.866025403784439,0.5,0.));
#8115=DIRECTION('ref_axis',(0.5,-0.866025403784439,0.));
#8116=DIRECTION('',(0.5,-0.866025403784439,8.97207371191609E-19));
#8117=DIRECTION('',(0.,0.,-1.));
#8118=DIRECTION('',(0.5,-0.866025403784439,0.));
#8119=DIRECTION('',(0.,0.,-1.));
#8120=DIRECTION('center_axis',(1.60246890531964E-16,1.,0.));
#8121=DIRECTION('ref_axis',(1.,-1.60246890531964E-16,0.));
#8122=DIRECTION('',(1.,-1.60246890531964E-16,9.78220653549071E-33));
#8123=DIRECTION('',(0.,0.,-1.));
#8124=DIRECTION('',(1.,-1.60246890531964E-16,0.));
#8125=DIRECTION('center_axis',(-0.866025403784438,0.5,0.));
#8126=DIRECTION('ref_axis',(0.5,0.866025403784438,0.));
#8127=DIRECTION('',(0.5,0.866025403784438,-8.97207371191599E-19));
#8128=DIRECTION('',(0.,0.,-1.));
#8129=DIRECTION('',(0.5,0.866025403784438,0.));
#8130=DIRECTION('center_axis',(-0.866025403784439,-0.499999999999999,0.));
#8131=DIRECTION('ref_axis',(-0.499999999999999,0.866025403784439,0.));
#8132=DIRECTION('',(-0.499999999999999,0.866025403784439,-8.97207371191609E-19));
#8133=DIRECTION('',(0.,0.,-1.));
#8134=DIRECTION('',(-0.499999999999999,0.866025403784439,0.));
#8135=DIRECTION('center_axis',(-1.60246890531964E-16,-1.,0.));
#8136=DIRECTION('ref_axis',(-1.,1.60246890531964E-16,0.));
#8137=DIRECTION('',(-1.,1.60246890531964E-16,-9.78220653549071E-33));
#8138=DIRECTION('',(0.,0.,-1.));
#8139=DIRECTION('',(-1.,1.60246890531964E-16,0.));
#8140=DIRECTION('center_axis',(0.866025403784439,-0.5,0.));
#8141=DIRECTION('ref_axis',(-0.5,-0.866025403784439,0.));
#8142=DIRECTION('',(-0.5,-0.866025403784439,8.97207371191599E-19));
#8143=DIRECTION('',(-0.5,-0.866025403784439,0.));
#8144=DIRECTION('center_axis',(0.,0.,-1.));
#8145=DIRECTION('ref_axis',(-1.,0.,0.));
#8146=DIRECTION('center_axis',(0.,0.,1.));
#8147=DIRECTION('ref_axis',(1.,0.,0.));
#8148=DIRECTION('center_axis',(0.,0.,-1.));
#8149=DIRECTION('ref_axis',(1.,0.,0.));
#8150=DIRECTION('',(0.,0.,-1.));
#8151=DIRECTION('center_axis',(0.,0.,1.));
#8152=DIRECTION('ref_axis',(1.,0.,0.));
#8153=DIRECTION('center_axis',(0.,0.,-1.));
#8154=DIRECTION('ref_axis',(1.,0.,0.));
#8155=DIRECTION('',(0.,0.,-1.));
#8156=DIRECTION('center_axis',(0.,0.,1.));
#8157=DIRECTION('ref_axis',(1.,0.,0.));
#8158=DIRECTION('center_axis',(0.,-1.,0.));
#8159=DIRECTION('ref_axis',(-1.,0.,0.));
#8160=DIRECTION('',(0.0523359562429438,0.,0.998629534754574));
#8161=DIRECTION('',(1.,0.,0.));
#8162=DIRECTION('',(-0.0523359562429438,0.,-0.998629534754574));
#8163=DIRECTION('',(1.,0.,0.));
#8164=DIRECTION('center_axis',(0.,-1.,0.));
#8165=DIRECTION('ref_axis',(-1.,0.,0.));
#8166=DIRECTION('',(0.,0.,-1.));
#8167=DIRECTION('',(1.,0.,0.));
#8168=DIRECTION('',(0.,0.,1.));
#8169=DIRECTION('',(1.,0.,0.));
#8170=DIRECTION('center_axis',(0.,-1.,0.));
#8171=DIRECTION('ref_axis',(-1.,0.,0.));
#8172=DIRECTION('',(0.,0.,-1.));
#8173=DIRECTION('',(1.,0.,0.));
#8174=DIRECTION('',(0.,0.,1.));
#8175=DIRECTION('',(1.,0.,0.));
#8176=DIRECTION('center_axis',(0.,-1.,0.));
#8177=DIRECTION('ref_axis',(-1.,0.,0.));
#8178=DIRECTION('',(0.,0.,-1.));
#8179=DIRECTION('',(1.,0.,0.));
#8180=DIRECTION('',(0.,0.,1.));
#8181=DIRECTION('',(1.,0.,0.));
#8182=DIRECTION('center_axis',(0.,1.,0.));
#8183=DIRECTION('ref_axis',(1.,0.,0.));
#8184=DIRECTION('',(-0.0523359562429438,0.,-0.998629534754574));
#8185=DIRECTION('',(-1.,0.,0.));
#8186=DIRECTION('',(0.0523359562429438,0.,0.998629534754574));
#8187=DIRECTION('',(-1.,0.,0.));
#8188=DIRECTION('center_axis',(0.,1.,0.));
#8189=DIRECTION('ref_axis',(1.,0.,0.));
#8190=DIRECTION('',(0.,0.,1.));
#8191=DIRECTION('',(-1.,0.,0.));
#8192=DIRECTION('',(0.,0.,-1.));
#8193=DIRECTION('',(-1.,0.,0.));
#8194=DIRECTION('center_axis',(0.,1.,0.));
#8195=DIRECTION('ref_axis',(1.,0.,0.));
#8196=DIRECTION('',(0.,0.,1.));
#8197=DIRECTION('',(-1.,0.,0.));
#8198=DIRECTION('',(0.,0.,-1.));
#8199=DIRECTION('',(-1.,0.,0.));
#8200=DIRECTION('center_axis',(0.,0.,1.));
#8201=DIRECTION('ref_axis',(1.,0.,0.));
#8202=DIRECTION('center_axis',(0.,0.,1.));
#8203=DIRECTION('ref_axis',(1.,0.,0.));
#8204=DIRECTION('center_axis',(0.,0.,1.));
#8205=DIRECTION('ref_axis',(1.,0.,0.));
#8206=DIRECTION('center_axis',(0.,0.,1.));
#8207=DIRECTION('ref_axis',(1.,0.,0.));
#8208=DIRECTION('center_axis',(0.,0.,1.));
#8209=DIRECTION('ref_axis',(1.,0.,0.));
#8210=DIRECTION('',(0.,1.,0.));
#8211=DIRECTION('',(0.,-1.,0.));
#8212=DIRECTION('center_axis',(0.,0.,1.));
#8213=DIRECTION('ref_axis',(1.,0.,0.));
#8214=DIRECTION('',(0.,-1.,0.));
#8215=DIRECTION('',(0.,1.,0.));
#8216=DIRECTION('center_axis',(0.,0.,1.));
#8217=DIRECTION('ref_axis',(1.,0.,0.));
#8218=DIRECTION('',(0.,-1.,0.));
#8219=DIRECTION('',(0.,1.,0.));
#8220=DIRECTION('center_axis',(0.,0.,1.));
#8221=DIRECTION('ref_axis',(1.,0.,0.));
#8222=DIRECTION('',(0.,-1.,0.));
#8223=DIRECTION('',(-1.,0.,0.));
#8224=DIRECTION('',(0.,1.,0.));
#8225=DIRECTION('center_axis',(0.,1.,0.));
#8226=DIRECTION('ref_axis',(1.,0.,0.));
#8227=DIRECTION('',(0.,0.,1.));
#8228=DIRECTION('',(-1.,0.,0.));
#8229=DIRECTION('',(0.,0.,-1.));
#8230=DIRECTION('center_axis',(-1.,0.,0.));
#8231=DIRECTION('ref_axis',(0.,-1.,0.));
#8232=DIRECTION('',(0.,-1.,0.));
#8233=DIRECTION('',(0.,-1.,1.03600583455278E-18));
#8234=DIRECTION('center_axis',(1.,0.,0.));
#8235=DIRECTION('ref_axis',(0.,1.,0.));
#8236=DIRECTION('',(0.,1.,0.));
#8237=DIRECTION('',(0.,1.,-1.03600583455278E-18));
#8238=DIRECTION('',(0.,1.,0.));
#8239=DIRECTION('center_axis',(1.,0.,0.));
#8240=DIRECTION('ref_axis',(0.,1.,0.));
#8241=DIRECTION('',(0.,1.,0.));
#8242=DIRECTION('',(0.,1.,-1.03600583455278E-18));
#8243=DIRECTION('',(0.,1.,0.));
#8244=DIRECTION('center_axis',(1.,0.,0.));
#8245=DIRECTION('ref_axis',(0.,1.,0.));
#8246=DIRECTION('',(0.,1.,0.));
#8247=DIRECTION('',(0.,1.,0.));
#8248=DIRECTION('center_axis',(0.998629534754574,0.,-0.0523359562429438));
#8249=DIRECTION('ref_axis',(-0.0523359562429438,0.,-0.998629534754574));
#8250=DIRECTION('',(0.,-1.,0.));
#8251=DIRECTION('',(5.42947651131849E-20,-1.,1.03600583455278E-18));
#8252=DIRECTION('',(0.,-1.,0.));
#8253=DIRECTION('center_axis',(0.,0.,1.));
#8254=DIRECTION('ref_axis',(1.,0.,0.));
#8255=DIRECTION('',(0.,-1.,0.));
#8256=DIRECTION('',(0.,-1.,0.));
#8257=DIRECTION('',(0.,-1.,0.));
#8258=DIRECTION('',(0.,1.,0.));
#8259=DIRECTION('',(0.,-1.,0.));
#8260=DIRECTION('',(0.,1.,0.));
#8261=DIRECTION('',(0.,-1.,0.));
#8262=DIRECTION('',(0.,-1.,0.));
#8263=DIRECTION('',(0.,-1.,0.));
#8264=DIRECTION('',(0.,1.,0.));
#8265=DIRECTION('',(0.,1.,0.));
#8266=DIRECTION('center_axis',(0.,0.,1.));
#8267=DIRECTION('ref_axis',(1.,0.,0.));
#8268=DIRECTION('center_axis',(-9.61618982193066E-33,1.03600583455278E-18,
1.));
#8269=DIRECTION('ref_axis',(1.,0.,0.));
#8270=DIRECTION('',(0.,0.,-1.));
#8271=DIRECTION('center_axis',(0.,0.,1.));
#8272=DIRECTION('ref_axis',(1.,0.,0.));
#8273=DIRECTION('',(0.,0.,-1.));
#8274=DIRECTION('center_axis',(1.,0.,0.));
#8275=DIRECTION('ref_axis',(0.,1.,0.));
#8276=DIRECTION('',(0.,1.,-1.03600583455278E-18));
#8277=DIRECTION('center_axis',(0.994044372876412,-0.108976074221552,-1.1933167131821E-14));
#8278=DIRECTION('ref_axis',(-0.108857570442347,-0.992963419871597,0.0466226999892957));
#8279=DIRECTION('center_axis',(-9.61618982193066E-33,1.03600583455278E-18,
1.));
#8280=DIRECTION('ref_axis',(1.,0.,9.61618982193066E-33));
#8281=DIRECTION('center_axis',(-9.61618982193066E-33,1.03600583455278E-18,
1.));
#8282=DIRECTION('ref_axis',(1.,0.,9.61618982193066E-33));
#8283=DIRECTION('',(-5.42947651131849E-20,-1.,1.03600583455278E-18));
#8284=DIRECTION('center_axis',(-1.,0.,0.));
#8285=DIRECTION('ref_axis',(0.,-1.,0.));
#8286=DIRECTION('',(0.,-1.,1.03600583455278E-18));
#8287=DIRECTION('center_axis',(-9.61618982193066E-33,1.03600583455278E-18,
1.));
#8288=DIRECTION('ref_axis',(1.,0.,9.61618982193066E-33));
#8289=DIRECTION('center_axis',(-1.,0.,0.));
#8290=DIRECTION('ref_axis',(0.,-1.,0.));
#8291=DIRECTION('center_axis',(-1.,0.,0.));
#8292=DIRECTION('ref_axis',(0.,-1.,0.));
#8293=DIRECTION('',(0.,-1.,1.03600583455278E-18));
#8294=DIRECTION('center_axis',(-0.999738255753194,0.0228783737088345,0.));
#8295=DIRECTION('ref_axis',(0.,0.,1.));
#8296=DIRECTION('center_axis',(-9.61618982193066E-33,1.03600583455278E-18,
1.));
#8297=DIRECTION('ref_axis',(1.,0.,9.61618982193066E-33));
#8298=DIRECTION('',(-5.42947651131849E-20,1.,-1.03600583455278E-18));
#8299=DIRECTION('center_axis',(-0.999738255790058,-0.0228783720979604,1.69987959829136E-9));
#8300=DIRECTION('ref_axis',(-0.022845652001536,0.998308458201847,0.0534630570326489));
#8301=DIRECTION('center_axis',(-0.375013085256251,-0.833398400631247,0.405970801550885));
#8302=DIRECTION('ref_axis',(-0.565498005067694,0.552672693214782,0.612180447612612));
#8303=DIRECTION('center_axis',(-7.78474640228738E-11,1.,0.));
#8304=DIRECTION('ref_axis',(0.,0.,1.));
#8305=DIRECTION('center_axis',(0.0522645732252412,-0.0522112666801462,0.997267465636596));
#8306=DIRECTION('ref_axis',(-0.998629534754574,0.,0.0523359562429445));
#8307=DIRECTION('center_axis',(0.361627795167438,-0.818371417997736,0.44664701943113));
#8308=DIRECTION('ref_axis',(0.514966362801186,0.574689674697898,0.636035708886648));
#8309=DIRECTION('center_axis',(0.994044372876412,0.108976074221546,-5.96658356591051E-15));
#8310=DIRECTION('ref_axis',(5.9211894646675E-15,7.40148683083438E-16,1.));
#8311=DIRECTION('center_axis',(-0.052263633556273,-0.0525535553916586,0.997249535684621));
#8312=DIRECTION('ref_axis',(-0.108857570442347,0.992963419871597,0.0466226999892949));
#8313=DIRECTION('center_axis',(0.,1.,0.));
#8314=DIRECTION('ref_axis',(0.998629534754574,0.,0.0523359562429438));
#8315=DIRECTION('center_axis',(0.375013085403515,-0.833398400816333,-0.405970801034895));
#8316=DIRECTION('ref_axis',(-0.565498005700927,-0.552672692935682,0.612180447279637));
#8317=DIRECTION('center_axis',(0.0522645732252408,0.0522112666801459,0.997267465636596));
#8318=DIRECTION('ref_axis',(-0.0228456520015352,-0.998308458201847,0.0534630570326489));
#8319=DIRECTION('center_axis',(-4.07418268117644E-12,-1.,-7.77400366303027E-11));
#8320=DIRECTION('ref_axis',(-0.998629534754574,0.,0.0523359562429438));
#8321=DIRECTION('center_axis',(-5.42947651131849E-20,1.,-1.03600583455278E-18));
#8322=DIRECTION('ref_axis',(-0.688354575693754,0.,0.725374371012288));
#8323=DIRECTION('center_axis',(-0.361627795167436,-0.818371417997736,-0.446647019431131));
#8324=DIRECTION('ref_axis',(0.514966362801185,-0.574689674697896,0.636035708886651));
#8325=DIRECTION('center_axis',(-0.0522636335562752,0.0525535553916633,0.99724953568462));
#8326=DIRECTION('ref_axis',(0.998629534754574,0.,0.0523359562429442));
#8327=DIRECTION('center_axis',(0.,-1.,0.));
#8328=DIRECTION('ref_axis',(0.,0.,1.));
#8329=DIRECTION('center_axis',(-5.42947651131849E-20,-1.,1.03600583455278E-18));
#8330=DIRECTION('ref_axis',(0.688354575693754,0.,0.725374371012288));
#8331=DIRECTION('',(5.42947651131849E-20,1.,-1.03600583455278E-18));
#8332=DIRECTION('center_axis',(-0.998629534754574,0.,-0.0523359562429438));
#8333=DIRECTION('ref_axis',(-0.0523359562429438,0.,0.998629534754574));
#8334=DIRECTION('center_axis',(-0.375013085256251,-0.833398400631247,0.405970801550885));
#8335=DIRECTION('ref_axis',(-0.565498005067695,0.552672693214781,0.612180447612612));
#8336=DIRECTION('center_axis',(-7.78474640228738E-11,1.,0.));
#8337=DIRECTION('ref_axis',(0.,0.,1.));
#8338=DIRECTION('center_axis',(-0.999738255790058,-0.0228783720979604,1.69987959829136E-9));
#8339=DIRECTION('ref_axis',(-0.022845652001536,0.998308458201847,0.0534630570326489));
#8340=DIRECTION('center_axis',(0.0522645732252412,-0.0522112666801462,0.997267465636596));
#8341=DIRECTION('ref_axis',(-0.998629534754574,0.,0.0523359562429445));
#8342=DIRECTION('center_axis',(0.361627795167442,-0.818371417997735,0.446647019431129));
#8343=DIRECTION('ref_axis',(0.514966362801186,0.574689674697898,0.636035708886649));
#8344=DIRECTION('center_axis',(0.994044372876412,0.108976074221546,-5.96658356591051E-15));
#8345=DIRECTION('ref_axis',(5.9211894646675E-15,7.40148683083438E-16,1.));
#8346=DIRECTION('center_axis',(0.,1.,0.));
#8347=DIRECTION('ref_axis',(0.998629534754574,0.,0.0523359562429438));
#8348=DIRECTION('center_axis',(-0.052263633556273,-0.0525535553916586,0.997249535684621));
#8349=DIRECTION('ref_axis',(-0.108857570442347,0.992963419871597,0.0466226999892949));
#8350=DIRECTION('center_axis',(0.375013085403515,-0.833398400816333,-0.405970801034895));
#8351=DIRECTION('ref_axis',(-0.565498005700926,-0.552672692935682,0.612180447279637));
#8352=DIRECTION('center_axis',(-0.999738255753194,0.0228783737088345,0.));
#8353=DIRECTION('ref_axis',(0.,0.,1.));
#8354=DIRECTION('center_axis',(-4.07418268117644E-12,-1.,-7.77400366303027E-11));
#8355=DIRECTION('ref_axis',(-0.998629534754574,0.,0.0523359562429438));
#8356=DIRECTION('center_axis',(0.0522645732252408,0.0522112666801459,0.997267465636596));
#8357=DIRECTION('ref_axis',(-0.0228456520015352,-0.998308458201847,0.0534630570326489));
#8358=DIRECTION('center_axis',(-5.42947651131849E-20,1.,-1.03600583455278E-18));
#8359=DIRECTION('ref_axis',(-0.688354575693754,0.,0.725374371012288));
#8360=DIRECTION('',(5.42947651131849E-20,-1.,1.03600583455278E-18));
#8361=DIRECTION('',(-5.42947651131849E-20,1.,-1.03600583455278E-18));
#8362=DIRECTION('center_axis',(-0.361627795167436,-0.818371417997736,-0.446647019431131));
#8363=DIRECTION('ref_axis',(0.51496636280118,-0.574689674697898,0.636035708886653));
#8364=DIRECTION('center_axis',(-0.0522636335562752,0.0525535553916633,0.99724953568462));
#8365=DIRECTION('ref_axis',(0.998629534754574,0.,0.0523359562429441));
#8366=DIRECTION('center_axis',(0.,-1.,0.));
#8367=DIRECTION('ref_axis',(0.,0.,1.));
#8368=DIRECTION('center_axis',(0.994044372876412,-0.108976074221552,-1.1933167131821E-14));
#8369=DIRECTION('ref_axis',(-0.108857570442347,-0.992963419871597,0.0466226999892957));
#8370=DIRECTION('center_axis',(-5.42947651131849E-20,-1.,1.03600583455278E-18));
#8371=DIRECTION('ref_axis',(0.688354575693754,0.,0.725374371012288));
#8372=DIRECTION('',(5.42947651131849E-20,1.,-1.03600583455278E-18));
#8373=DIRECTION('',(-5.42947651131849E-20,-1.,1.03600583455278E-18));
#8374=DIRECTION('center_axis',(0.998629534754574,0.,-0.0523359562429438));
#8375=DIRECTION('ref_axis',(-0.0523359562429438,0.,-0.998629534754574));
#8376=DIRECTION('center_axis',(-9.61618982193066E-33,1.03600583455278E-18,
1.));
#8377=DIRECTION('ref_axis',(1.,0.,9.61618982193066E-33));
#8378=DIRECTION('center_axis',(-0.998629534754574,0.,-0.0523359562429438));
#8379=DIRECTION('ref_axis',(-0.0523359562429438,0.,0.998629534754574));
#8380=DIRECTION('axis',(0.,0.,1.));
#8381=DIRECTION('refdir',(1.,0.,0.));
#8382=DIRECTION('center_axis',(0.,0.,-1.));
#8383=DIRECTION('ref_axis',(1.,0.,0.));
#8384=DIRECTION('center_axis',(-6.04309184969008E-32,-6.38489691472444E-32,
-1.));
#8385=DIRECTION('ref_axis',(1.,0.,0.));
#8386=DIRECTION('',(0.,0.,-1.));
#8387=DIRECTION('center_axis',(1.44549646912992E-31,1.50240180416177E-18,
1.));
#8388=DIRECTION('ref_axis',(1.,0.,0.));
#8389=DIRECTION('center_axis',(0.,0.,-1.));
#8390=DIRECTION('ref_axis',(1.,0.,0.));
#8391=DIRECTION('center_axis',(-6.04309184969008E-32,-6.38489691472444E-32,
-1.));
#8392=DIRECTION('ref_axis',(1.,0.,0.));
#8393=DIRECTION('',(0.,0.,-1.));
#8394=DIRECTION('center_axis',(1.44549646912992E-31,1.50240180416177E-18,
1.));
#8395=DIRECTION('ref_axis',(1.,0.,0.));
#8396=DIRECTION('center_axis',(0.,0.,1.));
#8397=DIRECTION('ref_axis',(1.,0.,0.));
#8398=DIRECTION('center_axis',(0.,0.,1.));
#8399=DIRECTION('ref_axis',(1.,0.,0.));
#8400=DIRECTION('center_axis',(0.,0.,-1.));
#8401=DIRECTION('ref_axis',(1.,0.,0.));
#8402=DIRECTION('center_axis',(0.,0.,-1.));
#8403=DIRECTION('ref_axis',(1.,0.,0.));
#8404=DIRECTION('center_axis',(0.,0.,-1.));
#8405=DIRECTION('ref_axis',(1.,0.,0.));
#8406=DIRECTION('',(0.,0.,1.));
#8407=DIRECTION('center_axis',(0.,0.,1.));
#8408=DIRECTION('ref_axis',(1.,0.,0.));
#8409=DIRECTION('center_axis',(0.,0.,1.));
#8410=DIRECTION('ref_axis',(1.,0.,0.));
#8411=DIRECTION('center_axis',(0.,0.,1.));
#8412=DIRECTION('ref_axis',(1.,0.,0.));
#8413=DIRECTION('center_axis',(0.,0.,-1.));
#8414=DIRECTION('ref_axis',(1.,0.,0.));
#8415=DIRECTION('center_axis',(0.,0.,-1.));
#8416=DIRECTION('ref_axis',(1.,0.,0.));
#8417=DIRECTION('center_axis',(0.,0.,-1.));
#8418=DIRECTION('ref_axis',(1.,0.,0.));
#8419=DIRECTION('',(0.,0.,1.));
#8420=DIRECTION('center_axis',(0.,0.,1.));
#8421=DIRECTION('ref_axis',(1.,0.,0.));
#8422=DIRECTION('center_axis',(0.,0.,1.));
#8423=DIRECTION('ref_axis',(1.,0.,0.));
#8424=DIRECTION('center_axis',(0.,0.,1.));
#8425=DIRECTION('ref_axis',(1.,0.,0.));
#8426=DIRECTION('center_axis',(0.,0.,-1.));
#8427=DIRECTION('ref_axis',(1.,0.,0.));
#8428=DIRECTION('center_axis',(0.,0.,-1.));
#8429=DIRECTION('ref_axis',(1.,0.,0.));
#8430=DIRECTION('center_axis',(0.,0.,-1.));
#8431=DIRECTION('ref_axis',(1.,0.,0.));
#8432=DIRECTION('',(0.,0.,1.));
#8433=DIRECTION('center_axis',(0.,0.,1.));
#8434=DIRECTION('ref_axis',(1.,0.,0.));
#8435=DIRECTION('center_axis',(0.,0.,1.));
#8436=DIRECTION('ref_axis',(1.,0.,0.));
#8437=DIRECTION('center_axis',(0.,0.,1.));
#8438=DIRECTION('ref_axis',(1.,0.,0.));
#8439=DIRECTION('center_axis',(0.,0.,-1.));
#8440=DIRECTION('ref_axis',(1.,0.,0.));
#8441=DIRECTION('center_axis',(0.,0.,-1.));
#8442=DIRECTION('ref_axis',(1.,0.,0.));
#8443=DIRECTION('center_axis',(0.,0.,-1.));
#8444=DIRECTION('ref_axis',(1.,0.,0.));
#8445=DIRECTION('',(0.,0.,1.));
#8446=DIRECTION('center_axis',(0.,0.,1.));
#8447=DIRECTION('ref_axis',(1.,0.,0.));
#8448=DIRECTION('center_axis',(0.,0.,-1.));
#8449=DIRECTION('ref_axis',(1.,0.,0.));
#8450=DIRECTION('',(0.,0.,1.));
#8451=DIRECTION('center_axis',(1.44549646912992E-31,1.50240180416177E-18,
1.));
#8452=DIRECTION('ref_axis',(1.,0.,0.));
#8453=DIRECTION('center_axis',(0.,0.,-1.));
#8454=DIRECTION('ref_axis',(1.,0.,0.));
#8455=DIRECTION('',(0.,0.,1.));
#8456=DIRECTION('center_axis',(1.44549646912992E-31,1.50240180416177E-18,
1.));
#8457=DIRECTION('ref_axis',(1.,0.,0.));
#8458=DIRECTION('center_axis',(0.,0.,-1.));
#8459=DIRECTION('ref_axis',(1.,0.,0.));
#8460=DIRECTION('',(0.,0.,1.));
#8461=DIRECTION('center_axis',(1.44549646912992E-31,1.50240180416177E-18,
1.));
#8462=DIRECTION('ref_axis',(1.,0.,0.));
#8463=DIRECTION('center_axis',(0.,0.,-1.));
#8464=DIRECTION('ref_axis',(1.,0.,0.));
#8465=DIRECTION('',(0.,0.,1.));
#8466=DIRECTION('center_axis',(1.44549646912992E-31,1.50240180416177E-18,
1.));
#8467=DIRECTION('ref_axis',(1.,0.,0.));
#8468=DIRECTION('center_axis',(0.,1.,0.));
#8469=DIRECTION('ref_axis',(0.,0.,1.));
#8470=DIRECTION('center_axis',(0.993165917563083,0.116711011438853,0.));
#8471=DIRECTION('ref_axis',(-0.116587207627638,0.992112394641407,0.0460480120795941));
#8472=DIRECTION('center_axis',(-3.34618268251883E-33,-1.,6.38489691472444E-32));
#8473=DIRECTION('ref_axis',(0.688354575693762,0.,0.72537437101228));
#8474=DIRECTION('center_axis',(0.,1.,0.));
#8475=DIRECTION('ref_axis',(0.,0.,1.));
#8476=DIRECTION('',(3.34618268251883E-33,1.,-6.38489691472444E-32));
#8477=DIRECTION('',(-3.34618268251883E-33,-1.,6.38489691472444E-32));
#8478=DIRECTION('center_axis',(0.993165917563077,-0.116711011438899,0.));
#8479=DIRECTION('ref_axis',(0.,0.,1.));
#8480=DIRECTION('center_axis',(0.999711469489423,-0.0240203615980049,0.));
#8481=DIRECTION('ref_axis',(0.,0.,1.));
#8482=DIRECTION('center_axis',(-3.69655756055634E-12,-1.,2.05200165779092E-26));
#8483=DIRECTION('ref_axis',(5.55111512312576E-15,0.,1.));
#8484=DIRECTION('center_axis',(-3.3461826825185E-33,1.,-6.38489691472444E-32));
#8485=DIRECTION('ref_axis',(-0.688354575693751,0.,0.72537437101229));
#8486=DIRECTION('center_axis',(0.,-1.,0.));
#8487=DIRECTION('ref_axis',(0.,0.,1.));
#8488=DIRECTION('',(3.3461826825185E-33,-1.,6.38489691472444E-32));
#8489=DIRECTION('',(-3.3461826825185E-33,1.,-6.38489691472444E-32));
#8490=DIRECTION('center_axis',(-0.999711469481833,-0.0240203619138888,2.77475672850144E-15));
#8491=DIRECTION('ref_axis',(2.77555756156288E-15,0.,1.));
#8492=DIRECTION('center_axis',(0.998629534754574,0.,-0.0523359562429439));
#8493=DIRECTION('ref_axis',(-0.0523359562429439,0.,-0.998629534754574));
#8494=DIRECTION('',(0.,1.,0.));
#8495=DIRECTION('center_axis',(6.04309184969008E-32,6.38489691472444E-32,
1.));
#8496=DIRECTION('ref_axis',(1.,0.,-6.04309184969008E-32));
#8497=DIRECTION('center_axis',(-0.998629534754574,0.,-0.0523359562429491));
#8498=DIRECTION('ref_axis',(-0.0523359562429491,0.,0.998629534754574));
#8499=DIRECTION('',(0.,-1.,0.));
#8500=DIRECTION('center_axis',(1.44549646912992E-31,1.50240180416177E-18,
1.));
#8501=DIRECTION('ref_axis',(1.,0.,-1.44549646912992E-31));
#8502=DIRECTION('axis',(0.,0.,1.));
#8503=DIRECTION('refdir',(1.,0.,0.));
#8504=DIRECTION('center_axis',(0.,0.,1.));
#8505=DIRECTION('ref_axis',(1.,0.,0.));
#8506=DIRECTION('',(0.,0.,-1.));
#8507=DIRECTION('center_axis',(0.,0.,-1.));
#8508=DIRECTION('ref_axis',(1.,0.,0.));
#8509=DIRECTION('center_axis',(0.,0.,1.));
#8510=DIRECTION('ref_axis',(1.,0.,0.));
#8511=DIRECTION('',(0.,0.,-1.));
#8512=DIRECTION('center_axis',(0.,0.,1.));
#8513=DIRECTION('ref_axis',(1.,0.,0.));
#8514=DIRECTION('',(0.,0.,-1.));
#8515=DIRECTION('center_axis',(0.,0.,1.));
#8516=DIRECTION('ref_axis',(1.,0.,0.));
#8517=DIRECTION('',(0.,0.,-1.));
#8518=DIRECTION('center_axis',(0.,0.,1.));
#8519=DIRECTION('ref_axis',(1.,0.,0.));
#8520=DIRECTION('',(0.,0.,-1.));
#8521=DIRECTION('center_axis',(0.,0.,1.));
#8522=DIRECTION('ref_axis',(1.,0.,0.));
#8523=DIRECTION('',(0.,0.,-1.));
#8524=DIRECTION('center_axis',(0.,0.,1.));
#8525=DIRECTION('ref_axis',(1.,0.,0.));
#8526=DIRECTION('',(0.,0.,-1.));
#8527=DIRECTION('center_axis',(0.,0.,1.));
#8528=DIRECTION('ref_axis',(1.,0.,0.));
#8529=DIRECTION('',(0.,0.,-1.));
#8530=DIRECTION('center_axis',(0.,0.,1.));
#8531=DIRECTION('ref_axis',(1.,0.,0.));
#8532=DIRECTION('',(0.,0.,-1.));
#8533=DIRECTION('center_axis',(0.,0.,1.));
#8534=DIRECTION('ref_axis',(1.,0.,0.));
#8535=DIRECTION('',(0.,0.,-1.));
#8536=DIRECTION('center_axis',(0.,0.,1.));
#8537=DIRECTION('ref_axis',(1.,0.,0.));
#8538=DIRECTION('',(0.,0.,-1.));
#8539=DIRECTION('center_axis',(0.,0.,1.));
#8540=DIRECTION('ref_axis',(1.,0.,0.));
#8541=DIRECTION('',(0.,0.,-1.));
#8542=DIRECTION('center_axis',(0.,0.,1.));
#8543=DIRECTION('ref_axis',(1.,0.,0.));
#8544=DIRECTION('',(0.,0.,-1.));
#8545=DIRECTION('center_axis',(0.,0.,1.));
#8546=DIRECTION('ref_axis',(1.,0.,0.));
#8547=DIRECTION('',(0.,0.,-1.));
#8548=DIRECTION('center_axis',(0.,0.,1.));
#8549=DIRECTION('ref_axis',(1.,0.,0.));
#8550=DIRECTION('',(0.,0.,-1.));
#8551=DIRECTION('center_axis',(0.,0.,1.));
#8552=DIRECTION('ref_axis',(1.,0.,0.));
#8553=DIRECTION('',(0.,0.,-1.));
#8554=DIRECTION('center_axis',(0.,0.,1.));
#8555=DIRECTION('ref_axis',(1.,0.,0.));
#8556=DIRECTION('',(0.,0.,-1.));
#8557=DIRECTION('center_axis',(0.,0.,1.));
#8558=DIRECTION('ref_axis',(1.,0.,0.));
#8559=DIRECTION('',(0.,0.,-1.));
#8560=DIRECTION('center_axis',(0.,0.,1.));
#8561=DIRECTION('ref_axis',(1.,0.,0.));
#8562=DIRECTION('',(0.,0.,-1.));
#8563=DIRECTION('center_axis',(0.,0.,1.));
#8564=DIRECTION('ref_axis',(1.,0.,0.));
#8565=DIRECTION('',(0.,0.,-1.));
#8566=DIRECTION('center_axis',(0.,0.,1.));
#8567=DIRECTION('ref_axis',(1.,0.,0.));
#8568=DIRECTION('',(0.,0.,-1.));
#8569=DIRECTION('center_axis',(0.,0.,1.));
#8570=DIRECTION('ref_axis',(1.,0.,0.));
#8571=DIRECTION('',(0.,0.,-1.));
#8572=DIRECTION('center_axis',(0.,0.,1.));
#8573=DIRECTION('ref_axis',(1.,0.,0.));
#8574=DIRECTION('',(0.,0.,-1.));
#8575=DIRECTION('center_axis',(0.,0.,1.));
#8576=DIRECTION('ref_axis',(1.,0.,0.));
#8577=DIRECTION('',(0.,0.,-1.));
#8578=DIRECTION('center_axis',(0.,0.,1.));
#8579=DIRECTION('ref_axis',(1.,0.,0.));
#8580=DIRECTION('',(0.,0.,-1.));
#8581=DIRECTION('center_axis',(0.,0.,1.));
#8582=DIRECTION('ref_axis',(1.,0.,0.));
#8583=DIRECTION('',(0.,0.,-1.));
#8584=DIRECTION('center_axis',(0.,0.,1.));
#8585=DIRECTION('ref_axis',(1.,0.,0.));
#8586=DIRECTION('',(0.,0.,-1.));
#8587=DIRECTION('center_axis',(0.,0.,1.));
#8588=DIRECTION('ref_axis',(1.,0.,0.));
#8589=DIRECTION('',(0.,0.,-1.));
#8590=DIRECTION('center_axis',(0.,0.,1.));
#8591=DIRECTION('ref_axis',(1.,0.,0.));
#8592=DIRECTION('',(0.,0.,-1.));
#8593=DIRECTION('center_axis',(0.,0.,1.));
#8594=DIRECTION('ref_axis',(1.,0.,0.));
#8595=DIRECTION('',(0.,0.,-1.));
#8596=DIRECTION('center_axis',(0.,0.,1.));
#8597=DIRECTION('ref_axis',(1.,-2.42503376499884E-13,0.));
#8598=DIRECTION('',(0.,0.,1.));
#8599=DIRECTION('center_axis',(0.,0.,-1.));
#8600=DIRECTION('ref_axis',(1.,-2.42503376499884E-13,0.));
#8601=DIRECTION('center_axis',(0.,0.,1.));
#8602=DIRECTION('ref_axis',(1.,-2.42503376499884E-13,0.));
#8603=DIRECTION('',(0.,0.,1.));
#8604=DIRECTION('center_axis',(0.,0.,1.));
#8605=DIRECTION('ref_axis',(1.,-2.42503376499884E-13,0.));
#8606=DIRECTION('',(0.,0.,1.));
#8607=DIRECTION('center_axis',(0.,0.,1.));
#8608=DIRECTION('ref_axis',(1.,-2.42503376499884E-13,0.));
#8609=DIRECTION('',(0.,0.,1.));
#8610=DIRECTION('center_axis',(0.,0.,1.));
#8611=DIRECTION('ref_axis',(1.,-2.42503376499884E-13,0.));
#8612=DIRECTION('',(0.,0.,1.));
#8613=DIRECTION('center_axis',(0.,0.,1.));
#8614=DIRECTION('ref_axis',(1.,-2.42503376499884E-13,0.));
#8615=DIRECTION('',(0.,0.,1.));
#8616=DIRECTION('center_axis',(0.,0.,1.));
#8617=DIRECTION('ref_axis',(1.,-2.42503376499884E-13,0.));
#8618=DIRECTION('',(0.,0.,1.));
#8619=DIRECTION('center_axis',(0.,0.,1.));
#8620=DIRECTION('ref_axis',(1.,-2.42503376499884E-13,0.));
#8621=DIRECTION('',(0.,0.,1.));
#8622=DIRECTION('center_axis',(0.,0.,1.));
#8623=DIRECTION('ref_axis',(1.,-2.42503376499884E-13,0.));
#8624=DIRECTION('',(0.,0.,1.));
#8625=DIRECTION('center_axis',(0.,0.,1.));
#8626=DIRECTION('ref_axis',(1.,-2.42503376499884E-13,0.));
#8627=DIRECTION('',(0.,0.,1.));
#8628=DIRECTION('center_axis',(0.,0.,1.));
#8629=DIRECTION('ref_axis',(1.,-2.42503376499884E-13,0.));
#8630=DIRECTION('',(0.,0.,1.));
#8631=DIRECTION('center_axis',(0.,0.,1.));
#8632=DIRECTION('ref_axis',(1.,-2.42503376499884E-13,0.));
#8633=DIRECTION('',(0.,0.,1.));
#8634=DIRECTION('center_axis',(0.,0.,1.));
#8635=DIRECTION('ref_axis',(1.,-2.42503376499884E-13,0.));
#8636=DIRECTION('',(0.,0.,1.));
#8637=DIRECTION('center_axis',(0.,0.,1.));
#8638=DIRECTION('ref_axis',(1.,-2.42503376499884E-13,0.));
#8639=DIRECTION('',(0.,0.,1.));
#8640=DIRECTION('center_axis',(0.,0.,1.));
#8641=DIRECTION('ref_axis',(1.,-2.42503376499884E-13,0.));
#8642=DIRECTION('',(0.,0.,1.));
#8643=DIRECTION('center_axis',(0.,0.,1.));
#8644=DIRECTION('ref_axis',(1.,-2.42503376499884E-13,0.));
#8645=DIRECTION('',(0.,0.,1.));
#8646=DIRECTION('center_axis',(0.,0.,1.));
#8647=DIRECTION('ref_axis',(1.,-2.42503376499884E-13,0.));
#8648=DIRECTION('',(0.,0.,1.));
#8649=DIRECTION('center_axis',(0.,0.,1.));
#8650=DIRECTION('ref_axis',(1.,-2.42503376499884E-13,0.));
#8651=DIRECTION('',(0.,0.,1.));
#8652=DIRECTION('center_axis',(0.,0.,1.));
#8653=DIRECTION('ref_axis',(1.,-2.42503376499884E-13,0.));
#8654=DIRECTION('',(0.,0.,1.));
#8655=DIRECTION('center_axis',(0.,0.,1.));
#8656=DIRECTION('ref_axis',(1.,-2.42503376499884E-13,0.));
#8657=DIRECTION('',(0.,0.,1.));
#8658=DIRECTION('center_axis',(0.,0.,1.));
#8659=DIRECTION('ref_axis',(1.,-2.42503376499884E-13,0.));
#8660=DIRECTION('',(0.,0.,1.));
#8661=DIRECTION('center_axis',(0.,0.,1.));
#8662=DIRECTION('ref_axis',(1.,-2.42503376499884E-13,0.));
#8663=DIRECTION('',(0.,0.,1.));
#8664=DIRECTION('center_axis',(0.,0.,1.));
#8665=DIRECTION('ref_axis',(1.,-2.42503376499884E-13,0.));
#8666=DIRECTION('',(0.,0.,1.));
#8667=DIRECTION('center_axis',(0.,0.,1.));
#8668=DIRECTION('ref_axis',(1.,-2.42503376499884E-13,0.));
#8669=DIRECTION('',(0.,0.,1.));
#8670=DIRECTION('center_axis',(0.,0.,1.));
#8671=DIRECTION('ref_axis',(1.,-2.42503376499884E-13,0.));
#8672=DIRECTION('',(0.,0.,1.));
#8673=DIRECTION('center_axis',(0.,0.,1.));
#8674=DIRECTION('ref_axis',(1.,-2.42503376499884E-13,0.));
#8675=DIRECTION('',(0.,0.,1.));
#8676=DIRECTION('center_axis',(0.,0.,1.));
#8677=DIRECTION('ref_axis',(1.,-2.42503376499884E-13,0.));
#8678=DIRECTION('',(0.,0.,1.));
#8679=DIRECTION('center_axis',(0.,0.,1.));
#8680=DIRECTION('ref_axis',(1.,-2.42503376499884E-13,0.));
#8681=DIRECTION('',(0.,0.,1.));
#8682=DIRECTION('center_axis',(0.,0.,1.));
#8683=DIRECTION('ref_axis',(1.,-2.42503376499884E-13,0.));
#8684=DIRECTION('',(0.,0.,1.));
#8685=DIRECTION('center_axis',(0.,0.,1.));
#8686=DIRECTION('ref_axis',(1.,-2.42503376499884E-13,0.));
#8687=DIRECTION('',(0.,0.,1.));
#8688=DIRECTION('center_axis',(0.,0.,-1.));
#8689=DIRECTION('ref_axis',(1.,0.,0.));
#8690=DIRECTION('center_axis',(0.,0.,-1.));
#8691=DIRECTION('ref_axis',(1.,0.,0.));
#8692=DIRECTION('',(0.707106781186547,8.65956056235493E-17,0.707106781186548));
#8693=DIRECTION('center_axis',(0.,0.,1.));
#8694=DIRECTION('ref_axis',(1.,0.,0.));
#8695=DIRECTION('center_axis',(0.,0.,1.));
#8696=DIRECTION('ref_axis',(1.,-2.42503376499884E-13,0.));
#8697=DIRECTION('center_axis',(0.,0.,-1.));
#8698=DIRECTION('ref_axis',(1.,-2.42503376499884E-13,0.));
#8699=DIRECTION('center_axis',(0.,0.,1.));
#8700=DIRECTION('ref_axis',(1.,0.,0.));
#8701=DIRECTION('center_axis',(-1.92296268638356E-16,-1.,0.));
#8702=DIRECTION('ref_axis',(1.,-1.92296268638356E-16,0.));
#8703=DIRECTION('',(1.,-1.92296268638356E-16,0.));
#8704=DIRECTION('',(0.,0.,1.));
#8705=DIRECTION('',(1.,-1.92296268638356E-16,0.));
#8706=DIRECTION('',(0.,0.,1.));
#8707=DIRECTION('center_axis',(-0.866025403784439,-0.5,0.));
#8708=DIRECTION('ref_axis',(0.5,-0.866025403784439,0.));
#8709=DIRECTION('',(0.5,-0.866025403784439,0.));
#8710=DIRECTION('',(0.,0.,1.));
#8711=DIRECTION('',(0.5,-0.866025403784439,0.));
#8712=DIRECTION('center_axis',(-0.866025403784439,0.5,0.));
#8713=DIRECTION('ref_axis',(-0.5,-0.866025403784439,0.));
#8714=DIRECTION('',(-0.5,-0.866025403784439,0.));
#8715=DIRECTION('',(0.,0.,1.));
#8716=DIRECTION('',(-0.5,-0.866025403784438,0.));
#8717=DIRECTION('center_axis',(1.92296268638356E-16,1.,0.));
#8718=DIRECTION('ref_axis',(-1.,1.92296268638356E-16,0.));
#8719=DIRECTION('',(-1.,1.92296268638356E-16,0.));
#8720=DIRECTION('',(0.,0.,1.));
#8721=DIRECTION('',(-1.,1.92296268638356E-16,0.));
#8722=DIRECTION('center_axis',(0.866025403784439,0.5,0.));
#8723=DIRECTION('ref_axis',(-0.5,0.866025403784439,0.));
#8724=DIRECTION('',(-0.5,0.866025403784439,0.));
#8725=DIRECTION('',(0.,0.,1.));
#8726=DIRECTION('',(-0.5,0.866025403784439,0.));
#8727=DIRECTION('center_axis',(0.866025403784439,-0.5,0.));
#8728=DIRECTION('ref_axis',(0.5,0.866025403784439,0.));
#8729=DIRECTION('',(0.5,0.866025403784439,0.));
#8730=DIRECTION('',(0.5,0.866025403784439,0.));
#8731=DIRECTION('center_axis',(0.,0.,1.));
#8732=DIRECTION('ref_axis',(1.,0.,0.));
#8733=DIRECTION('center_axis',(0.,0.,1.));
#8734=DIRECTION('ref_axis',(1.,0.,0.));
#8735=DIRECTION('center_axis',(0.,0.,1.));
#8736=DIRECTION('ref_axis',(1.,0.,0.));
#8737=DIRECTION('center_axis',(0.,0.,1.));
#8738=DIRECTION('ref_axis',(1.,0.,0.));
#8739=DIRECTION('',(0.,0.,-1.));
#8740=DIRECTION('center_axis',(0.,0.,1.));
#8741=DIRECTION('ref_axis',(1.,0.,0.));
#8742=DIRECTION('center_axis',(0.,0.,1.));
#8743=DIRECTION('ref_axis',(1.,0.,0.));
#8744=DIRECTION('center_axis',(0.,0.,1.));
#8745=DIRECTION('ref_axis',(1.,0.,0.));
#8746=DIRECTION('axis',(0.,0.,1.));
#8747=DIRECTION('refdir',(1.,0.,0.));
#8748=DIRECTION('center_axis',(0.,0.,-1.));
#8749=DIRECTION('ref_axis',(1.,0.,0.));
#8750=DIRECTION('',(0.,0.,-1.));
#8751=DIRECTION('center_axis',(0.,0.,-1.));
#8752=DIRECTION('ref_axis',(1.,0.,0.));
#8753=DIRECTION('center_axis',(0.,0.,-1.));
#8754=DIRECTION('ref_axis',(1.,0.,0.));
#8755=DIRECTION('',(0.,0.,-1.));
#8756=DIRECTION('center_axis',(0.,0.,-1.));
#8757=DIRECTION('ref_axis',(1.,0.,0.));
#8758=DIRECTION('center_axis',(0.,0.,-1.));
#8759=DIRECTION('ref_axis',(1.,0.,0.));
#8760=DIRECTION('',(0.,0.,-1.));
#8761=DIRECTION('center_axis',(0.,0.,-1.));
#8762=DIRECTION('ref_axis',(1.,0.,0.));
#8763=DIRECTION('',(0.,0.,-1.));
#8764=DIRECTION('center_axis',(0.,0.,-1.));
#8765=DIRECTION('ref_axis',(0.937385399639056,-0.348293859468591,0.));
#8766=DIRECTION('',(0.,0.,-1.));
#8767=DIRECTION('center_axis',(0.,0.,-1.));
#8768=DIRECTION('ref_axis',(1.,0.,0.));
#8769=DIRECTION('center_axis',(0.,0.,-1.));
#8770=DIRECTION('ref_axis',(0.28361887368566,0.958937085782627,0.));
#8771=DIRECTION('',(1.22464679914735E-16,8.07419868282478E-31,-1.));
#8772=DIRECTION('center_axis',(0.,0.,1.));
#8773=DIRECTION('ref_axis',(1.,6.71554824363804E-15,0.));
#8774=DIRECTION('center_axis',(0.,0.,-1.));
#8775=DIRECTION('ref_axis',(1.,6.71554824363804E-15,0.));
#8776=DIRECTION('',(1.22464679914735E-16,8.07419868282478E-31,-1.));
#8777=DIRECTION('center_axis',(0.,0.,-1.));
#8778=DIRECTION('ref_axis',(1.,6.71554824363804E-15,0.));
#8779=DIRECTION('',(1.22464679914735E-16,8.07419868282478E-31,-1.));
#8780=DIRECTION('center_axis',(0.,0.,-1.));
#8781=DIRECTION('ref_axis',(1.,6.71554824363804E-15,0.));
#8782=DIRECTION('',(1.22464679914735E-16,8.07419868282478E-31,-1.));
#8783=DIRECTION('center_axis',(0.,0.,-1.));
#8784=DIRECTION('ref_axis',(-0.60895050335979,-0.793208222636313,0.));
#8785=DIRECTION('',(1.22464679914735E-16,8.07419868282478E-31,-1.));
#8786=DIRECTION('center_axis',(0.,0.,-1.));
#8787=DIRECTION('ref_axis',(1.,6.71554824363804E-15,0.));
#8788=DIRECTION('center_axis',(0.,0.,-1.));
#8789=DIRECTION('ref_axis',(1.,6.71554824363804E-15,0.));
#8790=DIRECTION('center_axis',(0.,0.,1.));
#8791=DIRECTION('ref_axis',(1.,0.,0.));
#8792=DIRECTION('',(0.5,0.866025403784439,0.));
#8793=DIRECTION('',(-0.5,0.866025403784439,0.));
#8794=DIRECTION('',(-1.,0.,0.));
#8795=DIRECTION('',(-0.5,-0.866025403784439,0.));
#8796=DIRECTION('',(0.5,-0.866025403784439,0.));
#8797=DIRECTION('',(1.,-3.49629579342466E-16,0.));
#8798=DIRECTION('center_axis',(0.,0.,-1.));
#8799=DIRECTION('ref_axis',(1.,0.,0.));
#8800=DIRECTION('center_axis',(-3.49629579342466E-16,-1.,0.));
#8801=DIRECTION('ref_axis',(1.,-3.49629579342466E-16,0.));
#8802=DIRECTION('',(1.,-3.49629579342466E-16,0.));
#8803=DIRECTION('',(0.,0.,1.));
#8804=DIRECTION('',(0.,0.,1.));
#8805=DIRECTION('center_axis',(-0.866025403784439,-0.5,0.));
#8806=DIRECTION('ref_axis',(0.5,-0.866025403784439,0.));
#8807=DIRECTION('',(0.5,-0.866025403784439,0.));
#8808=DIRECTION('',(0.,0.,1.));
#8809=DIRECTION('center_axis',(-0.866025403784439,0.5,0.));
#8810=DIRECTION('ref_axis',(-0.5,-0.866025403784439,0.));
#8811=DIRECTION('',(-0.5,-0.866025403784439,0.));
#8812=DIRECTION('',(0.,0.,1.));
#8813=DIRECTION('center_axis',(0.,1.,0.));
#8814=DIRECTION('ref_axis',(-1.,0.,0.));
#8815=DIRECTION('',(-1.,0.,0.));
#8816=DIRECTION('',(0.,0.,1.));
#8817=DIRECTION('center_axis',(0.866025403784439,0.5,0.));
#8818=DIRECTION('ref_axis',(-0.5,0.866025403784439,0.));
#8819=DIRECTION('',(-0.5,0.866025403784439,0.));
#8820=DIRECTION('',(0.,0.,1.));
#8821=DIRECTION('center_axis',(0.866025403784439,-0.5,0.));
#8822=DIRECTION('ref_axis',(0.5,0.866025403784439,0.));
#8823=DIRECTION('',(0.5,0.866025403784439,0.));
#8824=DIRECTION('center_axis',(0.,0.,1.));
#8825=DIRECTION('ref_axis',(1.,0.,0.));
#8826=DIRECTION('',(0.,0.,1.));
#8827=DIRECTION('',(1.,0.,0.));
#8828=DIRECTION('',(0.,-1.22464679914735E-16,-1.));
#8829=DIRECTION('',(1.,0.,0.));
#8830=DIRECTION('',(0.,0.,1.));
#8831=DIRECTION('',(1.,0.,0.));
#8832=DIRECTION('',(0.,-1.22464679914735E-16,-1.));
#8833=DIRECTION('',(1.,0.,0.));
#8834=DIRECTION('',(0.,0.,1.));
#8835=DIRECTION('',(1.,0.,0.));
#8836=DIRECTION('',(0.,-1.22464679914735E-16,-1.));
#8837=DIRECTION('',(1.,0.,0.));
#8838=DIRECTION('',(0.,-1.22464679914735E-16,-1.));
#8839=DIRECTION('',(1.,0.,0.));
#8840=DIRECTION('',(0.,0.,1.));
#8841=DIRECTION('',(1.,0.,0.));
#8842=DIRECTION('axis',(0.,0.,1.));
#8843=DIRECTION('refdir',(1.,0.,0.));
#8844=DIRECTION('center_axis',(0.,0.,1.));
#8845=DIRECTION('ref_axis',(1.,0.,0.));
#8846=DIRECTION('center_axis',(0.,0.,-1.));
#8847=DIRECTION('ref_axis',(1.,0.,0.));
#8848=DIRECTION('',(0.,0.,-1.));
#8849=DIRECTION('center_axis',(0.,0.,-1.));
#8850=DIRECTION('ref_axis',(1.,0.,0.));
#8851=DIRECTION('center_axis',(0.,0.,1.));
#8852=DIRECTION('ref_axis',(1.,0.,0.));
#8853=DIRECTION('center_axis',(0.,0.,1.));
#8854=DIRECTION('ref_axis',(1.,0.,0.));
#8855=DIRECTION('',(0.,0.,-1.));
#8856=DIRECTION('center_axis',(0.,0.,1.));
#8857=DIRECTION('ref_axis',(1.,0.,0.));
#8858=DIRECTION('center_axis',(0.,0.,1.));
#8859=DIRECTION('ref_axis',(1.,0.,0.));
#8860=DIRECTION('center_axis',(0.,0.,1.));
#8861=DIRECTION('ref_axis',(1.,0.,0.));
#8862=DIRECTION('',(0.,0.,1.));
#8863=DIRECTION('',(1.,0.,0.));
#8864=DIRECTION('',(-6.12323401131865E-17,-1.22464679914735E-16,-1.));
#8865=DIRECTION('',(1.,3.46944695195361E-17,-6.12323401131864E-17));
#8866=DIRECTION('',(0.,0.,1.));
#8867=DIRECTION('',(1.,0.,0.));
#8868=DIRECTION('',(0.,0.,1.));
#8869=DIRECTION('',(1.,0.,0.));
#8870=DIRECTION('',(0.,0.,1.));
#8871=DIRECTION('',(1.,0.,0.));
#8872=DIRECTION('',(0.,0.,1.));
#8873=DIRECTION('',(1.,0.,0.));
#8874=DIRECTION('',(-6.12323401131865E-17,-1.22464679914735E-16,-1.));
#8875=DIRECTION('',(1.,3.46944695195361E-17,-6.12323401131864E-17));
#8876=DIRECTION('',(0.,0.,1.));
#8877=DIRECTION('',(1.,0.,0.));
#8878=CARTESIAN_POINT('',(0.,0.,0.));
#8879=CARTESIAN_POINT('',(0.,0.,0.));
#8880=CARTESIAN_POINT('Origin',(6.,-2.5,0.3));
#8881=CARTESIAN_POINT('',(5.83,-2.5,0.6));
#8882=CARTESIAN_POINT('Origin',(6.,-2.5,0.6));
#8883=CARTESIAN_POINT('',(5.83,-2.5,0.));
#8884=CARTESIAN_POINT('',(5.83,-2.5,0.3));
#8885=CARTESIAN_POINT('Origin',(6.,-2.5,0.));
#8886=CARTESIAN_POINT('Origin',(15.2,-2.5,0.3));
#8887=CARTESIAN_POINT('',(15.03,-2.5,0.6));
#8888=CARTESIAN_POINT('Origin',(15.2,-2.5,0.6));
#8889=CARTESIAN_POINT('',(15.03,-2.5,0.));
#8890=CARTESIAN_POINT('',(15.03,-2.5,0.3));
#8891=CARTESIAN_POINT('Origin',(15.2,-2.5,0.));
#8892=CARTESIAN_POINT('Origin',(0.,0.,0.3));
#8893=CARTESIAN_POINT('',(-0.41,5.02105187650415E-17,0.6));
#8894=CARTESIAN_POINT('Origin',(0.,0.,0.6));
#8895=CARTESIAN_POINT('',(-0.41,5.02105187650415E-17,0.));
#8896=CARTESIAN_POINT('',(-0.41,5.02105187650415E-17,0.3));
#8897=CARTESIAN_POINT('Origin',(0.,0.,0.));
#8898=CARTESIAN_POINT('Origin',(-2.,0.275,-0.175));
#8899=CARTESIAN_POINT('',(-2.,0.,0.));
#8900=CARTESIAN_POINT('',(-2.,0.,-0.3));
#8901=CARTESIAN_POINT('',(-2.,0.,-0.0875));
#8902=CARTESIAN_POINT('',(-2.,0.6,-0.3));
#8903=CARTESIAN_POINT('',(-2.,0.6,-0.3));
#8904=CARTESIAN_POINT('',(-2.,0.4875,-0.3));
#8905=CARTESIAN_POINT('Origin',(-5.7,0.6,-0.3));
#8906=CARTESIAN_POINT('',(-5.7,0.6,-0.3));
#8907=CARTESIAN_POINT('',(-5.7,0.,0.));
#8908=CARTESIAN_POINT('',(-5.7,0.6,-0.3));
#8909=CARTESIAN_POINT('',(-4.7,0.6,-0.3));
#8910=CARTESIAN_POINT('',(-5.75,0.,0.));
#8911=CARTESIAN_POINT('Origin',(-5.7,0.275,-0.175));
#8912=CARTESIAN_POINT('',(-5.7,0.,-0.3));
#8913=CARTESIAN_POINT('',(-5.7,0.,-0.0875));
#8914=CARTESIAN_POINT('',(-5.7,0.4875,-0.3));
#8915=CARTESIAN_POINT('Origin',(-5.8,0.,0.));
#8916=CARTESIAN_POINT('',(-1.6,0.,-0.3));
#8917=CARTESIAN_POINT('',(-1.6,0.,-0.3));
#8918=CARTESIAN_POINT('',(-1.6,0.,0.));
#8919=CARTESIAN_POINT('',(-1.6,0.,-0.3));
#8920=CARTESIAN_POINT('',(-1.4,0.,0.));
#8921=CARTESIAN_POINT('',(-1.2,0.,0.));
#8922=CARTESIAN_POINT('',(-1.4,0.,0.6));
#8923=CARTESIAN_POINT('',(-1.4,0.,0.));
#8924=CARTESIAN_POINT('',(-2.,0.,0.6));
#8925=CARTESIAN_POINT('',(-1.2,0.,0.6));
#8926=CARTESIAN_POINT('',(-2.,0.,0.1625));
#8927=CARTESIAN_POINT('Origin',(-2.,0.275,0.325));
#8928=CARTESIAN_POINT('',(-2.,0.6,0.6));
#8929=CARTESIAN_POINT('',(-2.,0.1375,0.6));
#8930=CARTESIAN_POINT('',(-2.,0.,0.));
#8931=CARTESIAN_POINT('Origin',(-5.7,0.,0.));
#8932=CARTESIAN_POINT('',(-5.7,0.6,0.6));
#8933=CARTESIAN_POINT('',(-5.7,0.,0.));
#8934=CARTESIAN_POINT('',(-2.85,0.6,0.6));
#8935=CARTESIAN_POINT('Origin',(-5.7,0.275,0.325));
#8936=CARTESIAN_POINT('',(-5.7,0.,0.6));
#8937=CARTESIAN_POINT('',(-5.7,0.1375,0.6));
#8938=CARTESIAN_POINT('',(-5.7,0.,0.1625));
#8939=CARTESIAN_POINT('Origin',(0.,0.,0.6));
#8940=CARTESIAN_POINT('',(0.518766934059614,-1.30033875129767,0.6));
#8941=CARTESIAN_POINT('Origin',(0.,0.,0.6));
#8942=CARTESIAN_POINT('',(3.8,-3.2,0.6));
#8943=CARTESIAN_POINT('',(0.,-1.,0.6));
#8944=CARTESIAN_POINT('',(16.4,-3.2,0.6));
#8945=CARTESIAN_POINT('',(3.8,-3.2,0.6));
#8946=CARTESIAN_POINT('',(16.4,-1.8,0.6));
#8947=CARTESIAN_POINT('',(16.4,-3.2,0.6));
#8948=CARTESIAN_POINT('',(3.8,-1.8,0.6));
#8949=CARTESIAN_POINT('',(16.4,-1.8,0.6));
#8950=CARTESIAN_POINT('',(1.,1.,0.6));
#8951=CARTESIAN_POINT('',(3.8,-1.8,0.6));
#8952=CARTESIAN_POINT('',(0.993295878967653,0.986591757935306,0.6));
#8953=CARTESIAN_POINT('',(1.,1.,0.6));
#8954=CARTESIAN_POINT('',(-1.2,0.721110255092798,0.6));
#8955=CARTESIAN_POINT('Origin',(0.,0.,0.6));
#8956=CARTESIAN_POINT('',(-1.2,1.4,0.6));
#8957=CARTESIAN_POINT('',(-1.2,1.4,0.6));
#8958=CARTESIAN_POINT('',(-3.,1.4,0.6));
#8959=CARTESIAN_POINT('',(-3.,1.4,0.6));
#8960=CARTESIAN_POINT('',(-5.8,0.6,0.6));
#8961=CARTESIAN_POINT('',(-5.8,0.6,0.6));
#8962=CARTESIAN_POINT('',(-5.8,0.,0.6));
#8963=CARTESIAN_POINT('',(-5.8,0.,0.6));
#8964=CARTESIAN_POINT('',(-1.2,0.,0.6));
#8965=CARTESIAN_POINT('Origin',(-1.6,0.,-0.3));
#8966=CARTESIAN_POINT('',(-1.6,1.4,-0.3));
#8967=CARTESIAN_POINT('',(-1.6,1.4,-0.3));
#8968=CARTESIAN_POINT('',(-1.6,1.4,0.));
#8969=CARTESIAN_POINT('',(-1.6,1.4,-0.3));
#8970=CARTESIAN_POINT('',(-1.6,0.,0.));
#8971=CARTESIAN_POINT('Origin',(-3.7,0.7,-0.3));
#8972=CARTESIAN_POINT('',(-5.8,0.,-0.3));
#8973=CARTESIAN_POINT('',(-1.6,0.,-0.3));
#8974=CARTESIAN_POINT('',(-5.8,0.6,-0.3));
#8975=CARTESIAN_POINT('',(-5.8,0.,-0.3));
#8976=CARTESIAN_POINT('',(-3.,1.4,-0.3));
#8977=CARTESIAN_POINT('',(-5.8,0.6,-0.3));
#8978=CARTESIAN_POINT('',(-3.,1.4,-0.3));
#8979=CARTESIAN_POINT('Origin',(-5.8,0.,0.));
#8980=CARTESIAN_POINT('',(-5.8,0.,0.));
#8981=CARTESIAN_POINT('Origin',(-1.2,0.,0.));
#8982=CARTESIAN_POINT('',(-1.2,0.721110255092798,0.));
#8983=CARTESIAN_POINT('',(-1.2,0.721110255092798,0.));
#8984=CARTESIAN_POINT('',(-1.2,1.4,0.));
#8985=CARTESIAN_POINT('',(-1.2,1.4,0.));
#8986=CARTESIAN_POINT('',(-1.2,1.4,0.));
#8987=CARTESIAN_POINT('Origin',(-5.8,0.6,0.));
#8988=CARTESIAN_POINT('',(-5.8,0.6,0.));
#8989=CARTESIAN_POINT('Origin',(-3.,1.4,0.));
#8990=CARTESIAN_POINT('',(-3.,1.4,0.));
#8991=CARTESIAN_POINT('Origin',(-1.2,1.4,0.));
#8992=CARTESIAN_POINT('',(-3.,1.4,0.));
#8993=CARTESIAN_POINT('Origin',(0.,0.,0.));
#8994=CARTESIAN_POINT('',(0.993295878967653,0.986591757935306,0.));
#8995=CARTESIAN_POINT('Origin',(0.,0.,0.));
#8996=CARTESIAN_POINT('',(1.,1.,0.));
#8997=CARTESIAN_POINT('',(1.,1.,0.));
#8998=CARTESIAN_POINT('',(3.8,-1.8,0.));
#8999=CARTESIAN_POINT('',(3.8,-1.8,0.));
#9000=CARTESIAN_POINT('',(16.4,-1.8,0.));
#9001=CARTESIAN_POINT('',(16.4,-1.8,0.));
#9002=CARTESIAN_POINT('',(16.4,-3.2,0.));
#9003=CARTESIAN_POINT('',(16.4,-3.2,0.));
#9004=CARTESIAN_POINT('',(3.8,-3.2,0.));
#9005=CARTESIAN_POINT('',(3.8,-3.2,0.));
#9006=CARTESIAN_POINT('',(0.518766934059614,-1.30033875129767,0.));
#9007=CARTESIAN_POINT('',(0.,-1.,0.));
#9008=CARTESIAN_POINT('Origin',(0.,0.,0.));
#9009=CARTESIAN_POINT('Origin',(0.,0.,0.));
#9010=CARTESIAN_POINT('',(0.993295878967653,0.986591757935306,0.));
#9011=CARTESIAN_POINT('Origin',(0.,-1.,0.));
#9012=CARTESIAN_POINT('',(0.518766934059614,-1.30033875129767,0.));
#9013=CARTESIAN_POINT('',(3.8,-3.2,0.));
#9014=CARTESIAN_POINT('Origin',(1.,1.,0.));
#9015=CARTESIAN_POINT('',(1.,1.,0.));
#9016=CARTESIAN_POINT('Origin',(3.8,-1.8,0.));
#9017=CARTESIAN_POINT('',(3.8,-1.8,0.));
#9018=CARTESIAN_POINT('Origin',(16.4,-1.8,0.));
#9019=CARTESIAN_POINT('',(16.4,-1.8,0.));
#9020=CARTESIAN_POINT('Origin',(16.4,-3.2,0.));
#9021=CARTESIAN_POINT('',(16.4,-3.2,0.));
#9022=CARTESIAN_POINT('Origin',(3.8,-3.2,0.));
#9023=CARTESIAN_POINT('Origin',(0.,0.,0.));
#9024=CARTESIAN_POINT('',(0.,0.,0.));
#9025=CARTESIAN_POINT('Origin',(6.,-2.5,0.3));
#9026=CARTESIAN_POINT('',(5.83,-2.5,0.6));
#9027=CARTESIAN_POINT('Origin',(6.,-2.5,0.6));
#9028=CARTESIAN_POINT('',(5.83,-2.5,0.));
#9029=CARTESIAN_POINT('',(5.83,-2.5,0.3));
#9030=CARTESIAN_POINT('Origin',(6.,-2.5,0.));
#9031=CARTESIAN_POINT('Origin',(15.2,-2.5,0.3));
#9032=CARTESIAN_POINT('',(15.03,-2.5,0.6));
#9033=CARTESIAN_POINT('Origin',(15.2,-2.5,0.6));
#9034=CARTESIAN_POINT('',(15.03,-2.5,0.));
#9035=CARTESIAN_POINT('',(15.03,-2.5,0.3));
#9036=CARTESIAN_POINT('Origin',(15.2,-2.5,0.));
#9037=CARTESIAN_POINT('Origin',(0.,0.,0.3));
#9038=CARTESIAN_POINT('',(-0.41,5.02105187650415E-17,0.6));
#9039=CARTESIAN_POINT('Origin',(0.,0.,0.6));
#9040=CARTESIAN_POINT('',(-0.41,5.02105187650415E-17,0.));
#9041=CARTESIAN_POINT('',(-0.41,5.02105187650415E-17,0.3));
#9042=CARTESIAN_POINT('Origin',(0.,0.,0.));
#9043=CARTESIAN_POINT('Origin',(-1.6,0.,-0.3));
#9044=CARTESIAN_POINT('',(-1.6,1.4,-0.3));
#9045=CARTESIAN_POINT('',(-1.6,0.,-0.3));
#9046=CARTESIAN_POINT('',(-1.6,1.4,-0.3));
#9047=CARTESIAN_POINT('',(-1.6,1.4,0.));
#9048=CARTESIAN_POINT('',(-1.6,1.4,-0.3));
#9049=CARTESIAN_POINT('',(-1.6,0.,0.));
#9050=CARTESIAN_POINT('',(-1.6,0.,0.));
#9051=CARTESIAN_POINT('',(-1.6,0.,-0.3));
#9052=CARTESIAN_POINT('Origin',(-3.7,0.7,-0.3));
#9053=CARTESIAN_POINT('',(-3.,1.4,-0.3));
#9054=CARTESIAN_POINT('',(-3.,1.4,-0.3));
#9055=CARTESIAN_POINT('',(-5.8,0.,-0.3));
#9056=CARTESIAN_POINT('',(-1.6,0.,-0.3));
#9057=CARTESIAN_POINT('',(-5.8,0.6,-0.3));
#9058=CARTESIAN_POINT('',(-5.8,0.,-0.3));
#9059=CARTESIAN_POINT('',(-5.8,0.6,-0.3));
#9060=CARTESIAN_POINT('Origin',(-5.8,0.,0.));
#9061=CARTESIAN_POINT('',(-1.4,0.,0.6));
#9062=CARTESIAN_POINT('',(-1.4,0.,0.));
#9063=CARTESIAN_POINT('',(-1.4,0.,0.));
#9064=CARTESIAN_POINT('',(-5.8,0.,0.6));
#9065=CARTESIAN_POINT('',(-1.2,0.,0.6));
#9066=CARTESIAN_POINT('',(-5.8,0.,0.));
#9067=CARTESIAN_POINT('',(-1.2,0.,0.));
#9068=CARTESIAN_POINT('Origin',(-1.2,0.,0.));
#9069=CARTESIAN_POINT('',(-1.2,0.721110255092798,0.));
#9070=CARTESIAN_POINT('',(-1.2,0.721110255092798,0.6));
#9071=CARTESIAN_POINT('',(-1.2,0.721110255092798,0.));
#9072=CARTESIAN_POINT('',(-1.2,1.4,0.));
#9073=CARTESIAN_POINT('',(-1.2,1.4,0.));
#9074=CARTESIAN_POINT('',(-1.2,1.4,0.6));
#9075=CARTESIAN_POINT('',(-1.2,1.4,0.));
#9076=CARTESIAN_POINT('',(-1.2,1.4,0.6));
#9077=CARTESIAN_POINT('Origin',(-5.8,0.6,0.));
#9078=CARTESIAN_POINT('',(-5.8,0.6,0.6));
#9079=CARTESIAN_POINT('',(-5.8,0.,0.6));
#9080=CARTESIAN_POINT('',(-5.8,0.6,0.));
#9081=CARTESIAN_POINT('Origin',(-3.,1.4,0.));
#9082=CARTESIAN_POINT('',(-3.,1.4,0.6));
#9083=CARTESIAN_POINT('',(-5.8,0.6,0.6));
#9084=CARTESIAN_POINT('',(-3.,1.4,0.));
#9085=CARTESIAN_POINT('Origin',(-1.2,1.4,0.));
#9086=CARTESIAN_POINT('',(-3.,1.4,0.6));
#9087=CARTESIAN_POINT('',(-3.,1.4,0.));
#9088=CARTESIAN_POINT('Origin',(0.,0.,0.));
#9089=CARTESIAN_POINT('',(0.993295878967653,0.986591757935306,0.));
#9090=CARTESIAN_POINT('Origin',(0.,0.,0.));
#9091=CARTESIAN_POINT('',(1.,1.,0.));
#9092=CARTESIAN_POINT('',(1.,1.,0.));
#9093=CARTESIAN_POINT('',(3.8,-1.8,0.));
#9094=CARTESIAN_POINT('',(3.8,-1.8,0.));
#9095=CARTESIAN_POINT('',(16.4,-1.8,0.));
#9096=CARTESIAN_POINT('',(16.4,-1.8,0.));
#9097=CARTESIAN_POINT('',(16.4,-3.2,0.));
#9098=CARTESIAN_POINT('',(16.4,-3.2,0.));
#9099=CARTESIAN_POINT('',(3.8,-3.2,0.));
#9100=CARTESIAN_POINT('',(3.8,-3.2,0.));
#9101=CARTESIAN_POINT('',(0.518766934059614,-1.30033875129767,0.));
#9102=CARTESIAN_POINT('',(0.,-1.,0.));
#9103=CARTESIAN_POINT('Origin',(0.,0.,0.));
#9104=CARTESIAN_POINT('Origin',(0.,0.,0.));
#9105=CARTESIAN_POINT('',(0.993295878967653,0.986591757935306,0.6));
#9106=CARTESIAN_POINT('Origin',(0.,0.,0.6));
#9107=CARTESIAN_POINT('',(0.993295878967653,0.986591757935306,0.));
#9108=CARTESIAN_POINT('Origin',(0.,-1.,0.));
#9109=CARTESIAN_POINT('',(0.518766934059614,-1.30033875129767,0.6));
#9110=CARTESIAN_POINT('',(0.518766934059614,-1.30033875129767,0.));
#9111=CARTESIAN_POINT('',(3.8,-3.2,0.6));
#9112=CARTESIAN_POINT('',(3.8,-3.2,0.));
#9113=CARTESIAN_POINT('',(0.,-1.,0.6));
#9114=CARTESIAN_POINT('Origin',(1.,1.,0.));
#9115=CARTESIAN_POINT('',(1.,1.,0.6));
#9116=CARTESIAN_POINT('',(1.,1.,0.6));
#9117=CARTESIAN_POINT('',(1.,1.,0.));
#9118=CARTESIAN_POINT('Origin',(3.8,-1.8,0.));
#9119=CARTESIAN_POINT('',(3.8,-1.8,0.6));
#9120=CARTESIAN_POINT('',(3.8,-1.8,0.6));
#9121=CARTESIAN_POINT('',(3.8,-1.8,0.));
#9122=CARTESIAN_POINT('Origin',(16.4,-1.8,0.));
#9123=CARTESIAN_POINT('',(16.4,-1.8,0.6));
#9124=CARTESIAN_POINT('',(16.4,-1.8,0.6));
#9125=CARTESIAN_POINT('',(16.4,-1.8,0.));
#9126=CARTESIAN_POINT('Origin',(16.4,-3.2,0.));
#9127=CARTESIAN_POINT('',(16.4,-3.2,0.6));
#9128=CARTESIAN_POINT('',(16.4,-3.2,0.6));
#9129=CARTESIAN_POINT('',(16.4,-3.2,0.));
#9130=CARTESIAN_POINT('Origin',(3.8,-3.2,0.));
#9131=CARTESIAN_POINT('',(3.8,-3.2,0.6));
#9132=CARTESIAN_POINT('Origin',(0.,0.,0.6));
#9133=CARTESIAN_POINT('Origin',(0.,0.,0.6));
#9134=CARTESIAN_POINT('Origin',(0.,0.,0.));
#9135=CARTESIAN_POINT('',(0.,0.,0.));
#9136=CARTESIAN_POINT('Origin',(0.,0.,0.75));
#9137=CARTESIAN_POINT('',(-0.3,-3.67394039744206E-17,0.7));
#9138=CARTESIAN_POINT('Origin',(0.,0.,0.7));
#9139=CARTESIAN_POINT('',(-0.3,-3.67394039744206E-17,0.8));
#9140=CARTESIAN_POINT('',(-0.3,-3.67394039744206E-17,0.75));
#9141=CARTESIAN_POINT('Origin',(0.,0.,0.8));
#9142=CARTESIAN_POINT('Origin',(0.7,0.,0.7));
#9143=CARTESIAN_POINT('',(-0.4,4.89858719658941E-17,0.7));
#9144=CARTESIAN_POINT('Origin',(0.,0.,0.7));
#9145=CARTESIAN_POINT('Origin',(0.3,0.,0.8));
#9146=CARTESIAN_POINT('',(-0.4,-4.89858719658941E-17,0.8));
#9147=CARTESIAN_POINT('Origin',(0.,0.,0.8));
#9148=CARTESIAN_POINT('Origin',(0.,0.,-0.7));
#9149=CARTESIAN_POINT('',(-0.4,-4.89858719658941E-17,0.9));
#9150=CARTESIAN_POINT('Origin',(0.,0.,0.9));
#9151=CARTESIAN_POINT('',(-0.4,-4.89858719658941E-17,-0.7));
#9152=CARTESIAN_POINT('Origin',(0.,0.,-0.7));
#9153=CARTESIAN_POINT('',(-0.6,-7.34788079488412E-17,-0.7));
#9154=CARTESIAN_POINT('Origin',(0.,0.,-0.7));
#9155=CARTESIAN_POINT('',(-0.4,-4.89858719658941E-17,-0.7));
#9156=CARTESIAN_POINT('Origin',(0.,0.,-0.7));
#9157=CARTESIAN_POINT('Origin',(0.,0.,-0.8));
#9158=CARTESIAN_POINT('',(-0.6,-7.34788079488412E-17,-0.8));
#9159=CARTESIAN_POINT('',(-0.6,-7.34788079488412E-17,-0.8));
#9160=CARTESIAN_POINT('Origin',(0.,0.,-0.8));
#9161=CARTESIAN_POINT('Origin',(0.,0.,-0.8));
#9162=CARTESIAN_POINT('Origin',(0.,0.,-0.7));
#9163=CARTESIAN_POINT('',(-0.4,-4.89858719658941E-17,-0.7));
#9164=CARTESIAN_POINT('Origin',(0.,0.,0.9));
#9165=CARTESIAN_POINT('',(0.,0.,0.));
#9166=CARTESIAN_POINT('Origin',(-0.1,0.,0.1));
#9167=CARTESIAN_POINT('',(-0.1,0.282842712474619,0.));
#9168=CARTESIAN_POINT('',(-0.1,0.282842712474619,0.1));
#9169=CARTESIAN_POINT('',(-0.1,0.282842712474619,0.));
#9170=CARTESIAN_POINT('',(-0.1,0.591607978309962,0.));
#9171=CARTESIAN_POINT('',(-0.1,0.,0.));
#9172=CARTESIAN_POINT('',(-0.1,0.591607978309962,0.1));
#9173=CARTESIAN_POINT('',(-0.1,0.591607978309962,0.));
#9174=CARTESIAN_POINT('',(-0.1,0.,0.1));
#9175=CARTESIAN_POINT('Origin',(0.1,1.2,0.1));
#9176=CARTESIAN_POINT('',(0.1,0.282842712474619,0.1));
#9177=CARTESIAN_POINT('',(0.1,0.282842712474619,0.));
#9178=CARTESIAN_POINT('',(0.1,0.282842712474619,0.));
#9179=CARTESIAN_POINT('',(0.1,0.591607978309962,0.1));
#9180=CARTESIAN_POINT('',(0.1,0.6,0.1));
#9181=CARTESIAN_POINT('',(0.1,0.591607978309962,0.));
#9182=CARTESIAN_POINT('',(0.1,0.591607978309962,0.));
#9183=CARTESIAN_POINT('',(0.1,0.6,0.));
#9184=CARTESIAN_POINT('Origin',(0.,0.,0.));
#9185=CARTESIAN_POINT('Origin',(0.,0.,0.));
#9186=CARTESIAN_POINT('Origin',(0.,0.,0.));
#9187=CARTESIAN_POINT('Origin',(0.,0.,0.));
#9188=CARTESIAN_POINT('Origin',(0.,0.,0.1));
#9189=CARTESIAN_POINT('Origin',(0.,0.,0.));
#9190=CARTESIAN_POINT('Origin',(0.,0.,0.1));
#9191=CARTESIAN_POINT('Origin',(0.,0.,0.1));
#9192=CARTESIAN_POINT('',(0.,0.,0.));
#9193=CARTESIAN_POINT('',(0.,0.,0.));
#9194=CARTESIAN_POINT('Origin',(6.87409734069396,-2.22251806091942E-16,
0.7));
#9195=CARTESIAN_POINT('',(3.31825992066485,1.2493322588334,0.7));
#9196=CARTESIAN_POINT('',(4.3,1.27917501057225,0.7));
#9197=CARTESIAN_POINT('Ctrl Pts',(3.31826243508713,1.24933270901874,0.7));
#9198=CARTESIAN_POINT('Ctrl Pts',(3.64552542112514,1.25866821321074,0.7));
#9199=CARTESIAN_POINT('Ctrl Pts',(3.97277304530853,1.26856018917077,0.7));
#9200=CARTESIAN_POINT('Ctrl Pts',(4.30000000005992,1.27917501058303,0.7));
#9201=CARTESIAN_POINT('',(4.3,-1.27917501057184,0.7));
#9202=CARTESIAN_POINT('',(4.3,0.742407407407408,0.7));
#9203=CARTESIAN_POINT('',(3.31825992075695,-1.24933225883136,0.7));
#9204=CARTESIAN_POINT('Ctrl Pts',(4.3000000000599,-1.27917501058303,0.7));
#9205=CARTESIAN_POINT('Ctrl Pts',(3.97277304533917,-1.26856018917177,0.7));
#9206=CARTESIAN_POINT('Ctrl Pts',(3.64552542118644,-1.25866821321259,0.7));
#9207=CARTESIAN_POINT('Ctrl Pts',(3.3182624351791,-1.24933270902137,0.7));
#9208=CARTESIAN_POINT('',(3.26759951430388,-1.24789152572578,0.7));
#9209=CARTESIAN_POINT('Ctrl Pts',(3.26760216044043,-1.24789199949781,0.7));
#9210=CARTESIAN_POINT('Ctrl Pts',(3.27154046708102,-1.24840675231115,0.699999999449966));
#9211=CARTESIAN_POINT('Ctrl Pts',(3.27549053112987,-1.2488275353013,0.699997549264952));
#9212=CARTESIAN_POINT('Ctrl Pts',(3.27944900419773,-1.24915404112413,0.699995443099811));
#9213=CARTESIAN_POINT('Ctrl Pts',(3.28202272903949,-1.24936632907779,0.699994073710794));
#9214=CARTESIAN_POINT('Ctrl Pts',(3.28459959180148,-1.24953872742098,0.699992815093061));
#9215=CARTESIAN_POINT('Ctrl Pts',(3.28717866899733,-1.24967118132558,0.699992046536556));
#9216=CARTESIAN_POINT('Ctrl Pts',(3.28888409507617,-1.24975876704947,0.699991538325205));
#9217=CARTESIAN_POINT('Ctrl Pts',(3.29059037034979,-1.2498288805585,0.699991238158591));
#9218=CARTESIAN_POINT('Ctrl Pts',(3.29229723346923,-1.24988151179005,0.69999118215758));
#9219=CARTESIAN_POINT('Ctrl Pts',(3.29393274317941,-1.24993194283473,0.699991128497625));
#9220=CARTESIAN_POINT('Ctrl Pts',(3.29556870469678,-1.24996631998408,0.699991298652463));
#9221=CARTESIAN_POINT('Ctrl Pts',(3.29720488848534,-1.24998463806557,0.699991673963628));
#9222=CARTESIAN_POINT('Ctrl Pts',(3.29943508678369,-1.25000960650399,0.699992185531049));
#9223=CARTESIAN_POINT('Ctrl Pts',(3.30166551218918,-1.25000473681137,0.699993084765318));
#9224=CARTESIAN_POINT('Ctrl Pts',(3.30389557412726,-1.24997002667259,0.699994176731177));
#9225=CARTESIAN_POINT('Ctrl Pts',(3.30868977915254,-1.24989540653807,0.699996524248132));
#9226=CARTESIAN_POINT('Ctrl Pts',(3.31348068594496,-1.24968290539118,0.699999999312134));
#9227=CARTESIAN_POINT('Ctrl Pts',(3.3182624351791,-1.24933270902137,0.7));
#9228=CARTESIAN_POINT('',(1.1,-1.19266190204492,0.7));
#9229=CARTESIAN_POINT('Ctrl Pts',(3.26760216044045,-1.24789199949781,0.7));
#9230=CARTESIAN_POINT('Ctrl Pts',(2.54512260523322,-1.2274084473838,0.7));
#9231=CARTESIAN_POINT('Ctrl Pts',(1.82256951666701,-1.20959509718369,0.7));
#9232=CARTESIAN_POINT('Ctrl Pts',(1.09999999999999,-1.19266190204553,0.7));
#9233=CARTESIAN_POINT('',(1.1,1.19266190204492,0.7));
#9234=CARTESIAN_POINT('',(1.1,-0.696450594095222,0.7));
#9235=CARTESIAN_POINT('',(3.26759952419083,1.24789152650872,0.7));
#9236=CARTESIAN_POINT('Ctrl Pts',(1.09999999999999,1.19266190204553,0.7));
#9237=CARTESIAN_POINT('Ctrl Pts',(1.82256951996781,1.20959509726105,0.7));
#9238=CARTESIAN_POINT('Ctrl Pts',(2.54512261183467,1.22740844754655,0.7));
#9239=CARTESIAN_POINT('Ctrl Pts',(3.26760217034162,1.24789199977852,0.7));
#9240=CARTESIAN_POINT('Ctrl Pts',(3.3182624351791,1.24933270902137,0.7));
#9241=CARTESIAN_POINT('Ctrl Pts',(3.3143012451848,1.2496228108833,0.699999999430174));
#9242=CARTESIAN_POINT('Ctrl Pts',(3.31033365565543,1.24981842655856,0.699997549220164));
#9243=CARTESIAN_POINT('Ctrl Pts',(3.30636302717881,1.24991943948955,0.699995443052606));
#9244=CARTESIAN_POINT('Ctrl Pts',(3.30378139908369,1.24998511620097,0.699994073661998));
#9245=CARTESIAN_POINT('Ctrl Pts',(3.3011989045204,1.25001078941611,0.699992815050698));
#9246=CARTESIAN_POINT('Ctrl Pts',(3.29861646861803,1.2499964568765,0.699992046505716));
#9247=CARTESIAN_POINT('Ctrl Pts',(3.2969088217217,1.24998697942277,0.699991538302026));
#9248=CARTESIAN_POINT('Ctrl Pts',(3.29520131971864,1.24996000972381,0.699991238145114));
#9249=CARTESIAN_POINT('Ctrl Pts',(3.29349422410899,1.24991555258537,0.699991182154076));
#9250=CARTESIAN_POINT('Ctrl Pts',(3.29185849176351,1.24987295392896,0.699991128503682));
#9251=CARTESIAN_POINT('Ctrl Pts',(3.29022322047391,1.2498143016413,0.699991298668259));
#9252=CARTESIAN_POINT('Ctrl Pts',(3.28858863969825,1.2497396036024,0.699991673987721));
#9253=CARTESIAN_POINT('Ctrl Pts',(3.286360626573,1.24963778654105,0.699992185566407));
#9254=CARTESIAN_POINT('Ctrl Pts',(3.28413408201674,1.24950616665997,0.699993084809042));
#9255=CARTESIAN_POINT('Ctrl Pts',(3.2819095957713,1.24934477520901,0.699994176777649));
#9256=CARTESIAN_POINT('Ctrl Pts',(3.27712738077041,1.24899781481787,0.699996524298861));
#9257=CARTESIAN_POINT('Ctrl Pts',(3.27235629258357,1.24851338385513,0.699999999330822));
#9258=CARTESIAN_POINT('Ctrl Pts',(3.26760217026193,1.24789200078152,0.699999999999999));
#9259=CARTESIAN_POINT('',(3.15,1.,0.7));
#9260=CARTESIAN_POINT('Origin',(3.3,1.,0.7));
#9261=CARTESIAN_POINT('',(3.15,-1.,0.7));
#9262=CARTESIAN_POINT('Origin',(3.3,-1.,0.7));
#9263=CARTESIAN_POINT('',(1.6,-4.89858719658941E-17,0.7));
#9264=CARTESIAN_POINT('Origin',(2.,0.,0.7));
#9265=CARTESIAN_POINT('Origin',(9.9,-1.,0.8));
#9266=CARTESIAN_POINT('',(9.75,-1.,0.9));
#9267=CARTESIAN_POINT('Origin',(9.9,-1.,0.9));
#9268=CARTESIAN_POINT('',(9.75,-1.,0.7));
#9269=CARTESIAN_POINT('',(9.75,-1.,0.8));
#9270=CARTESIAN_POINT('Origin',(9.9,-1.,0.7));
#9271=CARTESIAN_POINT('Origin',(3.3,-1.,0.8));
#9272=CARTESIAN_POINT('',(3.15,-1.,0.9));
#9273=CARTESIAN_POINT('Origin',(3.3,-1.,0.9));
#9274=CARTESIAN_POINT('',(3.15,-1.,0.8));
#9275=CARTESIAN_POINT('Origin',(3.3,1.,0.8));
#9276=CARTESIAN_POINT('',(3.15,1.,0.9));
#9277=CARTESIAN_POINT('Origin',(3.3,1.,0.9));
#9278=CARTESIAN_POINT('',(3.15,1.,0.8));
#9279=CARTESIAN_POINT('Origin',(9.9,1.,0.8));
#9280=CARTESIAN_POINT('',(9.75,1.,0.9));
#9281=CARTESIAN_POINT('Origin',(9.9,1.,0.9));
#9282=CARTESIAN_POINT('',(9.75,1.,0.7));
#9283=CARTESIAN_POINT('',(9.75,1.,0.8));
#9284=CARTESIAN_POINT('Origin',(9.9,1.,0.7));
#9285=CARTESIAN_POINT('Origin',(2.,0.,0.75));
#9286=CARTESIAN_POINT('',(1.7,3.67394039744206E-17,0.9));
#9287=CARTESIAN_POINT('Origin',(2.,0.,0.9));
#9288=CARTESIAN_POINT('',(1.7,3.67394039744206E-17,0.6));
#9289=CARTESIAN_POINT('',(1.7,3.67394039744206E-17,0.75));
#9290=CARTESIAN_POINT('Origin',(2.,0.,0.6));
#9291=CARTESIAN_POINT('Origin',(2.,0.,0.6));
#9292=CARTESIAN_POINT('',(1.83,-2.0818995585505E-17,0.6));
#9293=CARTESIAN_POINT('Origin',(2.,0.,0.6));
#9294=CARTESIAN_POINT('Origin',(11.2,0.,0.75));
#9295=CARTESIAN_POINT('',(10.9,3.67394039744206E-17,0.9));
#9296=CARTESIAN_POINT('Origin',(11.2,0.,0.9));
#9297=CARTESIAN_POINT('',(10.9,3.67394039744206E-17,0.6));
#9298=CARTESIAN_POINT('',(10.9,3.67394039744206E-17,0.75));
#9299=CARTESIAN_POINT('Origin',(11.2,0.,0.6));
#9300=CARTESIAN_POINT('Origin',(11.2,0.,0.6));
#9301=CARTESIAN_POINT('',(11.03,-2.0818995585505E-17,0.6));
#9302=CARTESIAN_POINT('Origin',(11.2,0.,0.6));
#9303=CARTESIAN_POINT('Origin',(2.,0.,0.45));
#9304=CARTESIAN_POINT('',(1.83,-2.0818995585505E-17,0.32));
#9305=CARTESIAN_POINT('',(1.83,2.0818995585505E-17,0.45));
#9306=CARTESIAN_POINT('Origin',(2.,0.,0.32));
#9307=CARTESIAN_POINT('Origin',(11.2,0.,0.45));
#9308=CARTESIAN_POINT('',(11.03,-2.0818995585505E-17,0.32));
#9309=CARTESIAN_POINT('',(11.03,2.0818995585505E-17,0.45));
#9310=CARTESIAN_POINT('Origin',(11.2,0.,0.32));
#9311=CARTESIAN_POINT('Origin',(12.4,-0.72,0.32));
#9312=CARTESIAN_POINT('',(0.200274469199584,-0.72,0.));
#9313=CARTESIAN_POINT('',(0.217044958570157,-0.72,0.32));
#9314=CARTESIAN_POINT('',(0.225070308370679,-0.72,0.473132796510599));
#9315=CARTESIAN_POINT('',(0.,-0.72,0.));
#9316=CARTESIAN_POINT('',(9.63649764092939,-0.72,0.));
#9317=CARTESIAN_POINT('',(0.0167704893705732,-0.72,0.32));
#9318=CARTESIAN_POINT('',(0.0253444014197637,-0.72,0.483599987759188));
#9319=CARTESIAN_POINT('',(-0.1,-0.72,0.32));
#9320=CARTESIAN_POINT('Origin',(12.4,-0.72,0.32));
#9321=CARTESIAN_POINT('',(0.9,-0.72,0.32));
#9322=CARTESIAN_POINT('',(0.9,-0.72,0.));
#9323=CARTESIAN_POINT('',(0.9,-0.72,0.16));
#9324=CARTESIAN_POINT('',(1.1,-0.72,0.32));
#9325=CARTESIAN_POINT('',(-0.1,-0.72,0.32));
#9326=CARTESIAN_POINT('',(1.1,-0.72,0.));
#9327=CARTESIAN_POINT('',(1.1,-0.72,0.16));
#9328=CARTESIAN_POINT('',(9.63649764092939,-0.72,0.));
#9329=CARTESIAN_POINT('Origin',(12.4,-0.72,0.32));
#9330=CARTESIAN_POINT('',(4.3,-0.72,0.32));
#9331=CARTESIAN_POINT('',(4.3,-0.72,0.));
#9332=CARTESIAN_POINT('',(4.3,-0.72,0.16));
#9333=CARTESIAN_POINT('',(4.5,-0.72,0.32));
#9334=CARTESIAN_POINT('',(-0.1,-0.72,0.32));
#9335=CARTESIAN_POINT('',(4.5,-0.72,0.));
#9336=CARTESIAN_POINT('',(4.5,-0.72,0.16));
#9337=CARTESIAN_POINT('',(9.63649764092939,-0.72,0.));
#9338=CARTESIAN_POINT('Origin',(12.4,-0.72,0.32));
#9339=CARTESIAN_POINT('',(8.7,-0.72,0.32));
#9340=CARTESIAN_POINT('',(8.7,-0.72,0.));
#9341=CARTESIAN_POINT('',(8.7,-0.72,0.16));
#9342=CARTESIAN_POINT('',(8.9,-0.72,0.32));
#9343=CARTESIAN_POINT('',(-0.1,-0.72,0.32));
#9344=CARTESIAN_POINT('',(8.9,-0.72,0.));
#9345=CARTESIAN_POINT('',(8.9,-0.72,0.16));
#9346=CARTESIAN_POINT('',(9.63649764092939,-0.72,0.));
#9347=CARTESIAN_POINT('Origin',(-0.0999999999999996,0.72,0.32));
#9348=CARTESIAN_POINT('',(0.217044958570158,0.72,0.32));
#9349=CARTESIAN_POINT('',(0.200274469199584,0.72,0.));
#9350=CARTESIAN_POINT('',(0.207951231396534,0.72,0.146481348799182));
#9351=CARTESIAN_POINT('',(0.0167704893705736,0.72,0.32));
#9352=CARTESIAN_POINT('',(12.4,0.72,0.32));
#9353=CARTESIAN_POINT('',(0.,0.72,0.));
#9354=CARTESIAN_POINT('',(0.00822532444561912,0.72,0.156948540047771));
#9355=CARTESIAN_POINT('',(3.38649764092939,0.72,0.));
#9356=CARTESIAN_POINT('Origin',(-0.0999999999999996,0.72,0.32));
#9357=CARTESIAN_POINT('',(0.9,0.72,0.));
#9358=CARTESIAN_POINT('',(0.9,0.72,0.32));
#9359=CARTESIAN_POINT('',(0.9,0.72,0.16));
#9360=CARTESIAN_POINT('',(1.1,0.72,0.));
#9361=CARTESIAN_POINT('',(3.38649764092939,0.72,0.));
#9362=CARTESIAN_POINT('',(1.1,0.72,0.32));
#9363=CARTESIAN_POINT('',(1.1,0.72,0.16));
#9364=CARTESIAN_POINT('',(12.4,0.72,0.32));
#9365=CARTESIAN_POINT('Origin',(-0.0999999999999996,0.72,0.32));
#9366=CARTESIAN_POINT('',(4.3,0.72,0.));
#9367=CARTESIAN_POINT('',(4.3,0.72,0.32));
#9368=CARTESIAN_POINT('',(4.3,0.72,0.16));
#9369=CARTESIAN_POINT('',(4.5,0.72,0.));
#9370=CARTESIAN_POINT('',(3.38649764092939,0.72,0.));
#9371=CARTESIAN_POINT('',(4.5,0.72,0.32));
#9372=CARTESIAN_POINT('',(4.5,0.72,0.16));
#9373=CARTESIAN_POINT('',(12.4,0.72,0.32));
#9374=CARTESIAN_POINT('Origin',(6.15,0.,0.32));
#9375=CARTESIAN_POINT('',(1.6,-4.89858719658941E-17,0.32));
#9376=CARTESIAN_POINT('Origin',(2.,0.,0.32));
#9377=CARTESIAN_POINT('Origin',(6.15,0.,0.32));
#9378=CARTESIAN_POINT('',(10.8,-4.89858719658942E-17,0.32));
#9379=CARTESIAN_POINT('Origin',(11.2,0.,0.32));
#9380=CARTESIAN_POINT('Origin',(6.15,0.,0.32));
#9381=CARTESIAN_POINT('',(0.217044958570157,-0.75,0.32));
#9382=CARTESIAN_POINT('',(0.0167704893705736,-0.75,0.32));
#9383=CARTESIAN_POINT('Origin',(6.15,0.,0.32));
#9384=CARTESIAN_POINT('',(0.9,0.696450594095222,0.32));
#9385=CARTESIAN_POINT('',(1.1,-0.696450594095222,0.32));
#9386=CARTESIAN_POINT('Origin',(6.15,0.,0.32));
#9387=CARTESIAN_POINT('',(4.3,0.742407407407408,0.32));
#9388=CARTESIAN_POINT('',(4.5,-0.742407407407408,0.32));
#9389=CARTESIAN_POINT('Origin',(6.15,0.,0.32));
#9390=CARTESIAN_POINT('',(8.7,0.72,0.32));
#9391=CARTESIAN_POINT('',(8.7,0.844259259259259,0.32));
#9392=CARTESIAN_POINT('',(8.9,0.72,0.32));
#9393=CARTESIAN_POINT('',(12.4,0.72,0.32));
#9394=CARTESIAN_POINT('',(8.9,-0.844259259259259,0.32));
#9395=CARTESIAN_POINT('Origin',(-0.0999999999999996,0.72,0.32));
#9396=CARTESIAN_POINT('',(8.7,0.72,0.));
#9397=CARTESIAN_POINT('',(8.7,0.72,0.16));
#9398=CARTESIAN_POINT('',(8.9,0.72,0.));
#9399=CARTESIAN_POINT('',(3.38649764092939,0.72,0.));
#9400=CARTESIAN_POINT('',(8.9,0.72,0.16));
#9401=CARTESIAN_POINT('Origin',(12.4,1.99376954809806,0.));
#9402=CARTESIAN_POINT('',(12.4,1.91212902562343,0.));
#9403=CARTESIAN_POINT('',(12.4,-1.91212902562343,0.));
#9404=CARTESIAN_POINT('',(12.4,1.99376954809806,0.));
#9405=CARTESIAN_POINT('',(12.4,-1.8833055216247,0.604732563714112));
#9406=CARTESIAN_POINT('Ctrl Pts',(12.4,-1.8833055216247,0.604732563714112));
#9407=CARTESIAN_POINT('Ctrl Pts',(12.4,-1.88809880980762,0.504101072758768));
#9408=CARTESIAN_POINT('Ctrl Pts',(12.4,-1.89289370245628,0.403468941627095));
#9409=CARTESIAN_POINT('Ctrl Pts',(12.4,-1.90250151416087,0.201891903194028));
#9410=CARTESIAN_POINT('Ctrl Pts',(12.4,-1.90731451170285,0.100945553925438));
#9411=CARTESIAN_POINT('Ctrl Pts',(12.4,-1.91212902562343,0.));
#9412=CARTESIAN_POINT('',(12.4,-1.78288409287054,0.7));
#9413=CARTESIAN_POINT('Ctrl Pts',(12.4000000030461,-1.78288409409899,0.7));
#9414=CARTESIAN_POINT('Ctrl Pts',(12.4000000066823,-1.79082830277209,0.699999997040196));
#9415=CARTESIAN_POINT('Ctrl Pts',(12.4000021328137,-1.79871128857748,0.699006690321208));
#9416=CARTESIAN_POINT('Ctrl Pts',(12.4000039827682,-1.8063921320806,0.697119229445379));
#9417=CARTESIAN_POINT('Ctrl Pts',(12.4000049365067,-1.81035196808589,0.69614615460905));
#9418=CARTESIAN_POINT('Ctrl Pts',(12.4000058167808,-1.81425808325963,0.694934510320783));
#9419=CARTESIAN_POINT('Ctrl Pts',(12.400006432968,-1.81808986884151,0.693492707237305));
#9420=CARTESIAN_POINT('Ctrl Pts',(12.4000076352846,-1.82556652433459,0.690679432664999));
#9421=CARTESIAN_POINT('Ctrl Pts',(12.4000076271954,-1.83268048852469,0.687023315130674));
#9422=CARTESIAN_POINT('Ctrl Pts',(12.4000063864816,-1.83928589538344,0.682605693351404));
#9423=CARTESIAN_POINT('Ctrl Pts',(12.4000055969106,-1.84348947395919,0.679794387301037));
#9424=CARTESIAN_POINT('Ctrl Pts',(12.400004329084,-1.84748689691167,0.676673627174617));
#9425=CARTESIAN_POINT('Ctrl Pts',(12.4000032503406,-1.8512341074341,0.673255429390325));
#9426=CARTESIAN_POINT('Ctrl Pts',(12.4000023796213,-1.85425870830395,0.670496394655072));
#9427=CARTESIAN_POINT('Ctrl Pts',(12.4000016297172,-1.85710218072175,0.667559826261508));
#9428=CARTESIAN_POINT('Ctrl Pts',(12.4000016274617,-1.859744520612,0.664455546516084));
#9429=CARTESIAN_POINT('Ctrl Pts',(12.4000016230979,-1.86485672743849,0.658449612092435));
#9430=CARTESIAN_POINT('Ctrl Pts',(12.4000041080363,-1.86921906069885,0.651817317967817));
#9431=CARTESIAN_POINT('Ctrl Pts',(12.40000495371,-1.8727702927896,0.64472299566344));
#9432=CARTESIAN_POINT('Ctrl Pts',(12.4000050555652,-1.8731980125259,0.643868536819953));
#9433=CARTESIAN_POINT('Ctrl Pts',(12.4000051394069,-1.87361391018412,0.643007349425002));
#9434=CARTESIAN_POINT('Ctrl Pts',(12.4000052029357,-1.87401783114888,0.642139703315781));
#9435=CARTESIAN_POINT('Ctrl Pts',(12.4000057294153,-1.87736522853405,0.634949295858174));
#9436=CARTESIAN_POINT('Ctrl Pts',(12.4000043880804,-1.87985460663586,0.627401584261416));
#9437=CARTESIAN_POINT('Ctrl Pts',(12.4000025112034,-1.88143175301701,0.619663949188762));
#9438=CARTESIAN_POINT('Ctrl Pts',(12.4000013193515,-1.88243327046239,0.614750406220363));
#9439=CARTESIAN_POINT('Ctrl Pts',(12.4,-1.88306607129604,0.609759643802656));
#9440=CARTESIAN_POINT('Ctrl Pts',(12.4,-1.8833055216247,0.604732563714112));
#9441=CARTESIAN_POINT('',(12.4,1.78288409287164,0.7));
#9442=CARTESIAN_POINT('',(12.4,0.99688477404903,0.7));
#9443=CARTESIAN_POINT('',(12.4,1.8833055216247,0.604732563714112));
#9444=CARTESIAN_POINT('Ctrl Pts',(12.4,1.8833055216247,0.604732563714112));
#9445=CARTESIAN_POINT('Ctrl Pts',(12.4,1.88292893537322,0.612638709665068));
#9446=CARTESIAN_POINT('Ctrl Pts',(12.4000029905988,1.88158186833012,0.620459457162159));
#9447=CARTESIAN_POINT('Ctrl Pts',(12.400004351969,1.87934739482834,0.62803467841275));
#9448=CARTESIAN_POINT('Ctrl Pts',(12.4000050124983,1.87826324073514,0.631710133556493));
#9449=CARTESIAN_POINT('Ctrl Pts',(12.4000053733669,1.87696936339782,0.63532777623417));
#9450=CARTESIAN_POINT('Ctrl Pts',(12.4000053391329,1.87547104796815,0.638868146717817));
#9451=CARTESIAN_POINT('Ctrl Pts',(12.4000052683671,1.872373843052,0.646186534188034));
#9452=CARTESIAN_POINT('Ctrl Pts',(12.4000032465668,1.86844110215533,0.653093304890266));
#9453=CARTESIAN_POINT('Ctrl Pts',(12.4000021327941,1.86374151467895,0.659427433016556));
#9454=CARTESIAN_POINT('Ctrl Pts',(12.4000018304335,1.86246569800928,0.66114698527342));
#9455=CARTESIAN_POINT('Ctrl Pts',(12.4000016226794,1.86113309763036,0.662824214875179));
#9456=CARTESIAN_POINT('Ctrl Pts',(12.400001625255,1.85974452038344,0.664455546516227));
#9457=CARTESIAN_POINT('Ctrl Pts',(12.4000016287814,1.85784336180007,0.666689070188443));
#9458=CARTESIAN_POINT('Ctrl Pts',(12.400002024929,1.85583728779192,0.668836587948716));
#9459=CARTESIAN_POINT('Ctrl Pts',(12.4000025639666,1.85373364862045,0.670894373083513));
#9460=CARTESIAN_POINT('Ctrl Pts',(12.400004021536,1.84804536272624,0.676458668669153));
#9461=CARTESIAN_POINT('Ctrl Pts',(12.4000062945443,1.84171268252251,0.681305055194542));
#9462=CARTESIAN_POINT('Ctrl Pts',(12.4000070319583,1.83490078417639,0.685381489016216));
#9463=CARTESIAN_POINT('Ctrl Pts',(12.4000075068619,1.8305138392177,0.688006761722114));
#9464=CARTESIAN_POINT('Ctrl Pts',(12.4000074483741,1.82592714021755,0.69031203082117));
#9465=CARTESIAN_POINT('Ctrl Pts',(12.4000068708525,1.82117863971551,0.692273867243687));
#9466=CARTESIAN_POINT('Ctrl Pts',(12.4000059767178,1.81382688138917,0.695311236040001));
#9467=CARTESIAN_POINT('Ctrl Pts',(12.4000038254996,1.80617119073902,0.697493343451155));
#9468=CARTESIAN_POINT('Ctrl Pts',(12.4000020685374,1.7983596509798,0.698751345219246));
#9469=CARTESIAN_POINT('Ctrl Pts',(12.4000009204513,1.79325520389048,0.699573385900268));
#9470=CARTESIAN_POINT('Ctrl Pts',(12.400000005426,1.78808359082883,0.699999998062804));
#9471=CARTESIAN_POINT('Ctrl Pts',(12.4000000030461,1.78288409409899,0.7));
#9472=CARTESIAN_POINT('Ctrl Pts',(12.4,1.91212902562343,0.));
#9473=CARTESIAN_POINT('Ctrl Pts',(12.4,1.90731404243129,0.1009553931071));
#9474=CARTESIAN_POINT('Ctrl Pts',(12.4,1.9025005759122,0.201911581737034));
#9475=CARTESIAN_POINT('Ctrl Pts',(12.4,1.89289276481806,0.403488620176902));
#9476=CARTESIAN_POINT('Ctrl Pts',(12.4,1.88809834114759,0.504110911924693));
#9477=CARTESIAN_POINT('Ctrl Pts',(12.4,1.8833055216247,0.604732563714112));
#9478=CARTESIAN_POINT('Origin',(8.9,-1.68851851851852,0.));
#9479=CARTESIAN_POINT('',(8.9,1.62420669932031,0.));
#9480=CARTESIAN_POINT('',(8.9,-1.68851851851852,0.));
#9481=CARTESIAN_POINT('',(8.9,1.59320117118329,0.605106081470792));
#9482=CARTESIAN_POINT('Ctrl Pts',(8.9,1.59320117118329,0.605106081470792));
#9483=CARTESIAN_POINT('Ctrl Pts',(8.9,1.59837103562161,0.504197738990529));
#9484=CARTESIAN_POINT('Ctrl Pts',(8.9,1.60354126123154,0.403288838380538));
#9485=CARTESIAN_POINT('Ctrl Pts',(8.9,1.61387642009944,0.201587196710533));
#9486=CARTESIAN_POINT('Ctrl Pts',(8.9,1.61904141157348,0.100793304842659));
#9487=CARTESIAN_POINT('Ctrl Pts',(8.9,1.62420669932031,0.));
#9488=CARTESIAN_POINT('',(8.9,1.49312521822106,0.7));
#9489=CARTESIAN_POINT('Ctrl Pts',(8.9,1.49312521822106,0.7));
#9490=CARTESIAN_POINT('Ctrl Pts',(8.9,1.50104136823484,0.7));
#9491=CARTESIAN_POINT('Ctrl Pts',(8.90000131173634,1.50889623314995,0.699007530025307));
#9492=CARTESIAN_POINT('Ctrl Pts',(8.90000245364087,1.51654949575132,0.697121675771258));
#9493=CARTESIAN_POINT('Ctrl Pts',(8.9000030153269,1.52031402289636,0.696194051841344));
#9494=CARTESIAN_POINT('Ctrl Pts',(8.90000353645954,1.52402976767023,0.695049421358208));
#9495=CARTESIAN_POINT('Ctrl Pts',(8.90000391188735,1.52767894577544,0.693695149285802));
#9496=CARTESIAN_POINT('Ctrl Pts',(8.90000468147812,1.53515940869299,0.690919022244083));
#9497=CARTESIAN_POINT('Ctrl Pts',(8.90000470661952,1.54227958804117,0.687295426711095));
#9498=CARTESIAN_POINT('Ctrl Pts',(8.9000039635008,1.54889410374269,0.682907715777054));
#9499=CARTESIAN_POINT('Ctrl Pts',(8.90000349228854,1.55308837416723,0.680125464281631));
#9500=CARTESIAN_POINT('Ctrl Pts',(8.90000272405863,1.55707914411963,0.677034908766328));
#9501=CARTESIAN_POINT('Ctrl Pts',(8.90000205379677,1.56082314136721,0.673648333128258));
#9502=CARTESIAN_POINT('Ctrl Pts',(8.90000149471997,1.56394607304962,0.670823532879853));
#9503=CARTESIAN_POINT('Ctrl Pts',(8.90000100172653,1.56687805273397,0.667809941545923));
#9504=CARTESIAN_POINT('Ctrl Pts',(8.90000100003,1.56959740049228,0.664618488856983));
#9505=CARTESIAN_POINT('Ctrl Pts',(8.90000099684156,1.57470809805256,0.658620525035968));
#9506=CARTESIAN_POINT('Ctrl Pts',(8.90000253934467,1.57907071782202,0.651995745956818));
#9507=CARTESIAN_POINT('Ctrl Pts',(8.90000305932469,1.58262507990443,0.644909256877938));
#9508=CARTESIAN_POINT('Ctrl Pts',(8.90000311559331,1.58300970826793,0.644142406277414));
#9509=CARTESIAN_POINT('Ctrl Pts',(8.9000031627798,1.58338482682255,0.643370127200485));
#9510=CARTESIAN_POINT('Ctrl Pts',(8.90000319981124,1.58375032531468,0.642592615892991));
#9511=CARTESIAN_POINT('Ctrl Pts',(8.90000354178946,1.58712563340961,0.635412448897651));
#9512=CARTESIAN_POINT('Ctrl Pts',(8.90000272882427,1.58964525157545,0.627871187463612));
#9513=CARTESIAN_POINT('Ctrl Pts',(8.90000156924769,1.59125549206429,0.620136848214628));
#9514=CARTESIAN_POINT('Ctrl Pts',(8.90000082792478,1.59228492658837,0.615192247765769));
#9515=CARTESIAN_POINT('Ctrl Pts',(8.89999999997262,1.59294182914154,0.610168076493048));
#9516=CARTESIAN_POINT('Ctrl Pts',(8.9000000009702,1.5932011715731,0.605106081469384));
#9517=CARTESIAN_POINT('',(8.9,-1.49312521822001,0.7));
#9518=CARTESIAN_POINT('',(8.9,-0.844259259259259,0.7));
#9519=CARTESIAN_POINT('',(8.9,-1.59320117118329,0.605106081470792));
#9520=CARTESIAN_POINT('Ctrl Pts',(8.90000000097019,-1.5932011715731,0.605106081469384));
#9521=CARTESIAN_POINT('Ctrl Pts',(8.89999999941083,-1.59279578158415,0.613018716877257));
#9522=CARTESIAN_POINT('Ctrl Pts',(8.90000185372291,-1.59142151714118,0.620841302874248));
#9523=CARTESIAN_POINT('Ctrl Pts',(8.90000269095591,-1.58916270068609,0.628413601005994));
#9524=CARTESIAN_POINT('Ctrl Pts',(8.90000316003867,-1.58789713677684,0.632656188846207));
#9525=CARTESIAN_POINT('Ctrl Pts',(8.90000337414869,-1.58635289833986,0.636820251299613));
#9526=CARTESIAN_POINT('Ctrl Pts',(8.90000326408749,-1.58453800492682,0.640875626603871));
#9527=CARTESIAN_POINT('Ctrl Pts',(8.9000030675631,-1.58129734600662,0.648116871770122));
#9528=CARTESIAN_POINT('Ctrl Pts',(8.90000169351568,-1.5772322800227,0.654932667693845));
#9529=CARTESIAN_POINT('Ctrl Pts',(8.90000116172667,-1.57240747726376,0.66116027211862));
#9530=CARTESIAN_POINT('Ctrl Pts',(8.90000106146602,-1.57149783490479,0.662334391157823));
#9531=CARTESIAN_POINT('Ctrl Pts',(8.90000099955281,-1.57056105641498,0.663487533005214));
#9532=CARTESIAN_POINT('Ctrl Pts',(8.90000100072893,-1.56959740053727,0.664618488856962));
#9533=CARTESIAN_POINT('Ctrl Pts',(8.9000010030487,-1.56769671285427,0.666849154291726));
#9534=CARTESIAN_POINT('Ctrl Pts',(8.90000124864079,-1.56569149899762,0.668993559652069));
#9535=CARTESIAN_POINT('Ctrl Pts',(8.90000158179872,-1.56358911460694,0.671047966011734));
#9536=CARTESIAN_POINT('Ctrl Pts',(8.90000248280001,-1.55790336961918,0.676603957919834));
#9537=CARTESIAN_POINT('Ctrl Pts',(8.90000387848177,-1.55157399841983,0.681441805123218));
#9538=CARTESIAN_POINT('Ctrl Pts',(8.90000432886686,-1.54476515293017,0.68550782533293));
#9539=CARTESIAN_POINT('Ctrl Pts',(8.9000046162921,-1.54041990676133,0.688102664467623));
#9540=CARTESIAN_POINT('Ctrl Pts',(8.90000458123012,-1.53587841548674,0.69038248607508));
#9541=CARTESIAN_POINT('Ctrl Pts',(8.90000422571091,-1.53117752164703,0.692323975790708));
#9542=CARTESIAN_POINT('Ctrl Pts',(8.90000367147839,-1.52384911813356,0.695350638493274));
#9543=CARTESIAN_POINT('Ctrl Pts',(8.9000023358238,-1.51621796414731,0.697522741667433));
#9544=CARTESIAN_POINT('Ctrl Pts',(8.90000125519218,-1.50843132129101,0.698770821080692));
#9545=CARTESIAN_POINT('Ctrl Pts',(8.90000055451733,-1.5033825102871,0.699580068042664));
#9546=CARTESIAN_POINT('Ctrl Pts',(8.9,-1.49826772866746,0.7));
#9547=CARTESIAN_POINT('Ctrl Pts',(8.9,-1.49312521822106,0.7));
#9548=CARTESIAN_POINT('',(8.9,-1.62420669932031,0.));
#9549=CARTESIAN_POINT('Ctrl Pts',(8.9,-1.62420669932031,0.));
#9550=CARTESIAN_POINT('Ctrl Pts',(8.9,-1.61904139377919,0.100793652073202));
#9551=CARTESIAN_POINT('Ctrl Pts',(8.9,-1.61387638451174,0.201587891198165));
#9552=CARTESIAN_POINT('Ctrl Pts',(8.9,-1.60354122564866,0.403289532862703));
#9553=CARTESIAN_POINT('Ctrl Pts',(8.9,-1.59837101783099,0.50419808623799));
#9554=CARTESIAN_POINT('Ctrl Pts',(8.9,-1.59320117118329,0.605106081470792));
#9555=CARTESIAN_POINT('',(8.9,-1.68851851851852,0.));
#9556=CARTESIAN_POINT('Origin',(4.5,-1.48481481481482,0.));
#9557=CARTESIAN_POINT('',(4.5,1.41772989878425,0.));
#9558=CARTESIAN_POINT('',(4.5,-1.48481481481482,0.));
#9559=CARTESIAN_POINT('',(4.5,1.38566996325095,0.605286533624017));
#9560=CARTESIAN_POINT('Ctrl Pts',(4.5,1.38566996325095,0.605286533624017));
#9561=CARTESIAN_POINT('Ctrl Pts',(4.5,1.3910232158183,0.504222354021684));
#9562=CARTESIAN_POINT('Ctrl Pts',(4.5,1.39637635187357,0.403158168247774));
#9563=CARTESIAN_POINT('Ctrl Pts',(4.5,1.4070629957395,0.201395990303158));
#9564=CARTESIAN_POINT('Ctrl Pts',(4.5,1.41239650438775,0.100697998177668));
#9565=CARTESIAN_POINT('Ctrl Pts',(4.5,1.41772989878425,0.));
#9566=CARTESIAN_POINT('',(4.5,1.28575421950843,0.7));
#9567=CARTESIAN_POINT('Ctrl Pts',(4.5,1.28575421950843,0.7));
#9568=CARTESIAN_POINT('Ctrl Pts',(4.5,1.29366545802379,0.7));
#9569=CARTESIAN_POINT('Ctrl Pts',(4.50000067540813,1.30151306508378,0.699006020085879));
#9570=CARTESIAN_POINT('Ctrl Pts',(4.50000126278178,1.30915682219698,0.697118891599074));
#9571=CARTESIAN_POINT('Ctrl Pts',(4.50000159346398,1.31346013814185,0.696056467716811));
#9572=CARTESIAN_POINT('Ctrl Pts',(4.50000189442328,1.31769890045703,0.694709922559592));
#9573=CARTESIAN_POINT('Ctrl Pts',(4.50000208642664,1.32184639782974,0.693090275295953));
#9574=CARTESIAN_POINT('Ctrl Pts',(4.50000243009859,1.32927011415192,0.690191225399894));
#9575=CARTESIAN_POINT('Ctrl Pts',(4.50000235826664,1.33632110693134,0.686451804482762));
#9576=CARTESIAN_POINT('Ctrl Pts',(4.50000192249634,1.34285330390028,0.681953677325188));
#9577=CARTESIAN_POINT('Ctrl Pts',(4.5000016824508,1.3464515866709,0.679475868782656));
#9578=CARTESIAN_POINT('Ctrl Pts',(4.50000134086274,1.34989218134371,0.676766953538005));
#9579=CARTESIAN_POINT('Ctrl Pts',(4.50000103767597,1.35314674504257,0.67383503027087));
#9580=CARTESIAN_POINT('Ctrl Pts',(4.50000074242034,1.35631617169348,0.670979804009792));
#9581=CARTESIAN_POINT('Ctrl Pts',(4.50000047986374,1.35928994516467,0.667930335702103));
#9582=CARTESIAN_POINT('Ctrl Pts',(4.5000004798165,1.36204555935344,0.66469809744354));
#9583=CARTESIAN_POINT('Ctrl Pts',(4.5000004797289,1.36715559606013,0.658704204607119));
#9584=CARTESIAN_POINT('Ctrl Pts',(4.50000128456446,1.3715183542993,0.652083197653858));
#9585=CARTESIAN_POINT('Ctrl Pts',(4.50000155892095,1.37507421485048,0.645000595057188));
#9586=CARTESIAN_POINT('Ctrl Pts',(4.50000158702893,1.37543851484667,0.644274978272754));
#9587=CARTESIAN_POINT('Ctrl Pts',(4.50000161091379,1.37579430519483,0.643544496675346));
#9588=CARTESIAN_POINT('Ctrl Pts',(4.50000163009343,1.37614149316233,0.642809317076966));
#9589=CARTESIAN_POINT('Ctrl Pts',(4.50000181728783,1.37953006709248,0.635633923185928));
#9590=CARTESIAN_POINT('Ctrl Pts',(4.50000140772507,1.38206400387968,0.628095594687559));
#9591=CARTESIAN_POINT('Ctrl Pts',(4.50000081194859,1.38368993781387,0.620362729373495));
#9592=CARTESIAN_POINT('Ctrl Pts',(4.50000042990035,1.38473258588096,0.615403944208116));
#9593=CARTESIAN_POINT('Ctrl Pts',(4.49999999988018,1.38540098970406,0.610364492806037));
#9594=CARTESIAN_POINT('Ctrl Pts',(4.50000000014037,1.38566996330298,0.605286533623957));
#9595=CARTESIAN_POINT('',(4.5,-1.28575421950842,0.7));
#9596=CARTESIAN_POINT('',(4.5,-0.742407407407408,0.7));
#9597=CARTESIAN_POINT('',(4.5,-1.38566996325095,0.605286533624017));
#9598=CARTESIAN_POINT('Ctrl Pts',(4.50000000014037,-1.38566996330298,0.605286533623957));
#9599=CARTESIAN_POINT('Ctrl Pts',(4.49999999973491,-1.38525081272033,0.613199687771457));
#9600=CARTESIAN_POINT('Ctrl Pts',(4.50000095642016,-1.38386419754969,0.62102180968747));
#9601=CARTESIAN_POINT('Ctrl Pts',(4.50000138305812,-1.38159414679432,0.628592503408469));
#9602=CARTESIAN_POINT('Ctrl Pts',(4.50000162118259,-1.38032713666619,0.632818023740444));
#9603=CARTESIAN_POINT('Ctrl Pts',(4.50000172745986,-1.37878391728058,0.636965253716347));
#9604=CARTESIAN_POINT('Ctrl Pts',(4.50000166716583,-1.37697237493585,0.641004309729874));
#9605=CARTESIAN_POINT('Ctrl Pts',(4.50000155916287,-1.37372741146613,0.648239354085419));
#9606=CARTESIAN_POINT('Ctrl Pts',(4.50000084040372,-1.36965973349804,0.655049237033139));
#9607=CARTESIAN_POINT('Ctrl Pts',(4.50000056390271,-1.36483316768901,0.661270759279915));
#9608=CARTESIAN_POINT('Ctrl Pts',(4.50000051219424,-1.36393055121024,0.662434246679675));
#9609=CARTESIAN_POINT('Ctrl Pts',(4.50000048023544,-1.3630012658104,0.663577087492372));
#9610=CARTESIAN_POINT('Ctrl Pts',(4.50000048056391,-1.36204555937839,0.664698097443534));
#9611=CARTESIAN_POINT('Ctrl Pts',(4.50000048121673,-1.36014610273268,0.666926093123284));
#9612=CARTESIAN_POINT('Ctrl Pts',(4.50000060829837,-1.35814231322364,0.669067903674665));
#9613=CARTESIAN_POINT('Ctrl Pts',(4.50000078085101,-1.35604151212276,0.671119765431539));
#9614=CARTESIAN_POINT('Ctrl Pts',(4.50000124774248,-1.3503571825734,0.676671675324794));
#9615=CARTESIAN_POINT('Ctrl Pts',(4.50000197143062,-1.34402953514766,0.681505303070731));
#9616=CARTESIAN_POINT('Ctrl Pts',(4.50000220836427,-1.33722229030693,0.685566265232058));
#9617=CARTESIAN_POINT('Ctrl Pts',(4.50000235894787,-1.33289593407788,0.688147216755564));
#9618=CARTESIAN_POINT('Ctrl Pts',(4.50000234488938,-1.32837489877041,0.690415387400166));
#9619=CARTESIAN_POINT('Ctrl Pts',(4.50000216490635,-1.32369554581057,0.69234752884452));
#9620=CARTESIAN_POINT('Ctrl Pts',(4.50000188343739,-1.31637767466938,0.695369135087455));
#9621=CARTESIAN_POINT('Ctrl Pts',(4.50000119588393,-1.3087575932273,0.697536490026807));
#9622=CARTESIAN_POINT('Ctrl Pts',(4.50000064127173,-1.30098224657147,0.698779892333419));
#9623=CARTESIAN_POINT('Ctrl Pts',(4.50000028296845,-1.29595903898196,0.699583183579437));
#9624=CARTESIAN_POINT('Ctrl Pts',(4.5,-1.29087043558603,0.7));
#9625=CARTESIAN_POINT('Ctrl Pts',(4.5,-1.28575421950843,0.7));
#9626=CARTESIAN_POINT('',(4.5,-1.41772989878425,0.));
#9627=CARTESIAN_POINT('Ctrl Pts',(4.5,-1.41772989878425,0.));
#9628=CARTESIAN_POINT('Ctrl Pts',(4.5,-1.41239649634988,0.100698149937961));
#9629=CARTESIAN_POINT('Ctrl Pts',(4.5,-1.40706297966336,0.201396293824709));
#9630=CARTESIAN_POINT('Ctrl Pts',(4.5,-1.39637633579674,0.403158471769294));
#9631=CARTESIAN_POINT('Ctrl Pts',(4.5,-1.39102320777973,0.504222505781934));
#9632=CARTESIAN_POINT('Ctrl Pts',(4.5,-1.38566996325095,0.605286533624017));
#9633=CARTESIAN_POINT('',(4.5,-1.48481481481482,0.));
#9634=CARTESIAN_POINT('Origin',(1.1,-1.39290118819044,0.));
#9635=CARTESIAN_POINT('',(1.1,1.324891758307,0.));
#9636=CARTESIAN_POINT('',(1.1,-1.39290118819044,0.));
#9637=CARTESIAN_POINT('',(1.10000000295569,1.29254692766489,0.605334652628491));
#9638=CARTESIAN_POINT('Ctrl Pts',(1.10000000295569,1.29254692766489,0.605334652628491));
#9639=CARTESIAN_POINT('Ctrl Pts',(1.10000000295569,1.29794978210809,0.504228164786351));
#9640=CARTESIAN_POINT('Ctrl Pts',(1.1,1.30335245345465,0.403121008362245));
#9641=CARTESIAN_POINT('Ctrl Pts',(1.1,1.31413403739463,0.20134322693425));
#9642=CARTESIAN_POINT('Ctrl Pts',(1.1,1.31951302132877,0.100671299071668));
#9643=CARTESIAN_POINT('Ctrl Pts',(1.1,1.324891758307,0.));
#9644=CARTESIAN_POINT('Ctrl Pts',(1.1,1.19266190204553,0.7));
#9645=CARTESIAN_POINT('Ctrl Pts',(1.1,1.20057109129252,0.7));
#9646=CARTESIAN_POINT('Ctrl Pts',(1.10000046829629,1.20841685974333,0.699006220526237));
#9647=CARTESIAN_POINT('Ctrl Pts',(1.10000087277688,1.21605887983377,0.697119382842322));
#9648=CARTESIAN_POINT('Ctrl Pts',(1.10000109992184,1.22035042410288,0.696059787689036));
#9649=CARTESIAN_POINT('Ctrl Pts',(1.10000130563842,1.22457776983048,0.694717521940989));
#9650=CARTESIAN_POINT('Ctrl Pts',(1.10000143498593,1.22871439246446,0.693103507978966));
#9651=CARTESIAN_POINT('Ctrl Pts',(1.10000166711622,1.23613807995602,0.690206957744321));
#9652=CARTESIAN_POINT('Ctrl Pts',(1.10000160692769,1.24318920265812,0.686469797174223));
#9653=CARTESIAN_POINT('Ctrl Pts',(1.10000129432656,1.24972159507123,0.681973692132557));
#9654=CARTESIAN_POINT('Ctrl Pts',(1.10000112259081,1.25331033895651,0.679503636989594));
#9655=CARTESIAN_POINT('Ctrl Pts',(1.10000088087184,1.25674225826706,0.676803638555143));
#9656=CARTESIAN_POINT('Ctrl Pts',(1.10000066684112,1.25998923415267,0.673881729486736));
#9657=CARTESIAN_POINT('Ctrl Pts',(1.100000457217,1.26316935916797,0.671019978599686));
#9658=CARTESIAN_POINT('Ctrl Pts',(1.1000002715704,1.26615273734033,0.667962699881477));
#9659=CARTESIAN_POINT('Ctrl Pts',(1.1000002731257,1.2689166530284,0.664721467295484));
#9660=CARTESIAN_POINT('Ctrl Pts',(1.10000027600127,1.2740268283512,0.658728785663437));
#9661=CARTESIAN_POINT('Ctrl Pts',(1.10000085014601,1.27838972527875,0.652108677049879));
#9662=CARTESIAN_POINT('Ctrl Pts',(1.1000010530947,1.28194599975408,0.64502688444408));
#9663=CARTESIAN_POINT('Ctrl Pts',(1.10000107362034,1.2823056710724,0.644310652415237));
#9664=CARTESIAN_POINT('Ctrl Pts',(1.10000109127028,1.28265705236355,0.643589678557342));
#9665=CARTESIAN_POINT('Ctrl Pts',(1.10000110571348,1.28300005475086,0.642864123553892));
#9666=CARTESIAN_POINT('Ctrl Pts',(1.10000124853573,1.28639184812822,0.635689442715943));
#9667=CARTESIAN_POINT('Ctrl Pts',(1.10000097361067,1.28892914698194,0.628151301589031));
#9668=CARTESIAN_POINT('Ctrl Pts',(1.10000056283738,1.29055881622654,0.620418355899457));
#9669=CARTESIAN_POINT('Ctrl Pts',(1.10000029930222,1.29160434466024,0.615457217544876));
#9670=CARTESIAN_POINT('Ctrl Pts',(1.0999999999818,1.29227543558766,0.610415225971447));
#9671=CARTESIAN_POINT('Ctrl Pts',(1.1000000000255,1.29254692753179,0.605334652628598));
#9672=CARTESIAN_POINT('',(1.10000000295569,-1.29254692766489,0.605334652628491));
#9673=CARTESIAN_POINT('Ctrl Pts',(1.1000000000255,-1.29254692753179,0.605334652628598));
#9674=CARTESIAN_POINT('Ctrl Pts',(1.09999999995744,-1.29212405100831,0.613248166229861));
#9675=CARTESIAN_POINT('Ctrl Pts',(1.10000066442022,-1.29073420569755,0.621070584654331));
#9676=CARTESIAN_POINT('Ctrl Pts',(1.10000095378343,-1.28846118610397,0.628641296001913));
#9677=CARTESIAN_POINT('Ctrl Pts',(1.10000111506646,-1.28719426797524,0.632861000698125));
#9678=CARTESIAN_POINT('Ctrl Pts',(1.10000118318417,-1.28565198202118,0.637002542581089));
#9679=CARTESIAN_POINT('Ctrl Pts',(1.10000113489265,-1.28384214455607,0.641036116698538));
#9680=CARTESIAN_POINT('Ctrl Pts',(1.10000104828677,-1.28059638744501,0.648269916488365));
#9681=CARTESIAN_POINT('Ctrl Pts',(1.10000053334783,-1.27652829029495,0.655078571385522));
#9682=CARTESIAN_POINT('Ctrl Pts',(1.10000033433257,-1.27170133822839,0.661298646557671));
#9683=CARTESIAN_POINT('Ctrl Pts',(1.10000029715544,-1.27079963749419,0.662460590217389));
#9684=CARTESIAN_POINT('Ctrl Pts',(1.10000027400485,-1.26987132743055,0.663601924550879));
#9685=CARTESIAN_POINT('Ctrl Pts',(1.10000027368829,-1.26891665304159,0.664721467295481));
#9686=CARTESIAN_POINT('Ctrl Pts',(1.10000027305905,-1.2670190620795,0.666946764442229));
#9687=CARTESIAN_POINT('Ctrl Pts',(1.10000036187052,-1.26501734165944,0.669086014589825));
#9688=CARTESIAN_POINT('Ctrl Pts',(1.10000048327469,-1.26291879257262,0.671135465892351));
#9689=CARTESIAN_POINT('Ctrl Pts',(1.10000081209565,-1.25723491092676,0.676686367091516));
#9690=CARTESIAN_POINT('Ctrl Pts',(1.10000132622062,-1.25090760500066,0.68151881845922));
#9691=CARTESIAN_POINT('Ctrl Pts',(1.10000150097561,-1.24410063152763,0.68557843671136));
#9692=CARTESIAN_POINT('Ctrl Pts',(1.10000161196703,-1.2397773464179,0.688156805381407));
#9693=CARTESIAN_POINT('Ctrl Pts',(1.1000016084534,-1.23525961544019,0.690422742497405));
#9694=CARTESIAN_POINT('Ctrl Pts',(1.10000148831111,-1.23058375131837,0.692353039195786));
#9695=CARTESIAN_POINT('Ctrl Pts',(1.10000130031927,-1.22326722442338,0.695373457954986));
#9696=CARTESIAN_POINT('Ctrl Pts',(1.1000008264887,-1.21564857658641,0.697539632783775));
#9697=CARTESIAN_POINT('Ctrl Pts',(1.10000044322439,-1.20787483729518,0.698781928831272));
#9698=CARTESIAN_POINT('Ctrl Pts',(1.1000001958084,-1.20285650563037,0.6995838921283));
#9699=CARTESIAN_POINT('Ctrl Pts',(1.1,-1.19777295102175,0.7));
#9700=CARTESIAN_POINT('Ctrl Pts',(1.1,-1.19266190204553,0.7));
#9701=CARTESIAN_POINT('',(1.1,-1.324891758307,0.));
#9702=CARTESIAN_POINT('Ctrl Pts',(1.1,-1.324891758307,0.));
#9703=CARTESIAN_POINT('Ctrl Pts',(1.1,-1.3195129727271,0.10067220872632));
#9704=CARTESIAN_POINT('Ctrl Pts',(1.1,-1.31413394019217,0.201345046154956));
#9705=CARTESIAN_POINT('Ctrl Pts',(1.1,-1.30335235623932,0.40312282767794));
#9706=CARTESIAN_POINT('Ctrl Pts',(1.10000000295569,-1.29794973349953,0.504229074424201));
#9707=CARTESIAN_POINT('Ctrl Pts',(1.10000000295569,-1.29254692766489,0.605334652628491));
#9708=CARTESIAN_POINT('',(1.1,-1.39290118819044,0.));
#9709=CARTESIAN_POINT('Origin',(0.199725906950915,-1.5,-0.0104671912485888));
#9710=CARTESIAN_POINT('',(0.200274469199584,1.20659878095028,0.));
#9711=CARTESIAN_POINT('',(0.200274469199585,-0.75,0.));
#9712=CARTESIAN_POINT('',(0.231993417893744,1.17491202960101,0.605233595624295));
#9713=CARTESIAN_POINT('Ctrl Pts',(0.200274469199584,1.20659878095028,-9.43255890062389E-18));
#9714=CARTESIAN_POINT('Ctrl Pts',(0.210847451958254,1.19603647956141,0.20174452921517));
#9715=CARTESIAN_POINT('Ctrl Pts',(0.221420434855641,1.18547422886796,0.403489061077219));
#9716=CARTESIAN_POINT('Ctrl Pts',(0.231993417893744,1.17491202960101,0.605233595624295));
#9717=CARTESIAN_POINT('',(0.231993417893744,-1.17491202960101,0.605233595624295));
#9718=CARTESIAN_POINT('',(0.231993417893744,-0.75,0.605233595624295));
#9719=CARTESIAN_POINT('',(0.200274469199584,-1.20659878095028,1.38777878078145E-17));
#9720=CARTESIAN_POINT('Ctrl Pts',(0.231993417893744,-1.17491202960101,0.605233595624295));
#9721=CARTESIAN_POINT('Ctrl Pts',(0.221420434855641,-1.18547422886796,0.40348906107722));
#9722=CARTESIAN_POINT('Ctrl Pts',(0.210847451958254,-1.19603647956141,0.20174452921517));
#9723=CARTESIAN_POINT('Ctrl Pts',(0.200274469199584,-1.20659878095028,2.0491421059976E-17));
#9724=CARTESIAN_POINT('',(0.200274469199585,-0.75,0.));
#9725=CARTESIAN_POINT('Origin',(6.87299528185878,-3.57834294608796E-18,
0.));
#9726=CARTESIAN_POINT('Ctrl Pts',(8.90000000000001,-1.62420669932031,-3.75133951679985E-17));
#9727=CARTESIAN_POINT('Ctrl Pts',(10.0682843079684,-1.69891080436391,-1.31961514553165E-7));
#9728=CARTESIAN_POINT('Ctrl Pts',(11.2345361392062,-1.79243531443695,-6.44452192334729E-8));
#9729=CARTESIAN_POINT('Ctrl Pts',(12.4000000002382,-1.91212902541327,2.95121624705651E-11));
#9730=CARTESIAN_POINT('Ctrl Pts',(12.4000000002382,1.91212902541327,2.95118849063386E-11));
#9731=CARTESIAN_POINT('Ctrl Pts',(11.2345361911441,1.79243531977099,-6.4445136166539E-8));
#9732=CARTESIAN_POINT('Ctrl Pts',(10.0682843567552,1.69891080748336,-1.31958638870612E-7));
#9733=CARTESIAN_POINT('Ctrl Pts',(8.9,1.62420669932031,6.39679281766448E-17));
#9734=CARTESIAN_POINT('',(8.7,1.61160179736194,0.));
#9735=CARTESIAN_POINT('',(8.7,1.68851851851852,0.));
#9736=CARTESIAN_POINT('Ctrl Pts',(8.70000000002062,1.61160179731554,-3.21507306454832E-13));
#9737=CARTESIAN_POINT('Ctrl Pts',(7.99734938728961,1.56795839277283,5.29471456843263E-9));
#9738=CARTESIAN_POINT('Ctrl Pts',(7.29393815910572,1.53097060499506,-6.44604909847991E-9));
#9739=CARTESIAN_POINT('Ctrl Pts',(6.58949465297818,1.49904250536939,-7.60372244394637E-9));
#9740=CARTESIAN_POINT('Ctrl Pts',(5.94302350041144,1.46974193664425,-8.66612477447903E-9));
#9741=CARTESIAN_POINT('Ctrl Pts',(5.29757001768168,1.44478244743454,1.79883147367388E-8));
#9742=CARTESIAN_POINT('Ctrl Pts',(4.65216233480351,1.42284617839366,3.84107779578714E-9));
#9743=CARTESIAN_POINT('Ctrl Pts',(4.60144142975536,1.4211222642714,2.72928337404163E-9));
#9744=CARTESIAN_POINT('Ctrl Pts',(4.55072080855761,1.41941704699729,1.44770501019496E-9));
#9745=CARTESIAN_POINT('Ctrl Pts',(4.50000000001737,1.41772989873549,-1.00876616052154E-12));
#9746=CARTESIAN_POINT('',(4.3,1.41116952203211,0.));
#9747=CARTESIAN_POINT('',(4.3,1.48481481481482,0.));
#9748=CARTESIAN_POINT('Ctrl Pts',(4.3,1.41116952203211,-1.0790522121662E-15));
#9749=CARTESIAN_POINT('Ctrl Pts',(3.23514221724601,1.37672428690534,3.20725535317031E-8));
#9750=CARTESIAN_POINT('Ctrl Pts',(2.16992716239601,1.34987955958158,4.63097810372671E-9));
#9751=CARTESIAN_POINT('Ctrl Pts',(1.10000000020726,1.32489175811528,-9.82792569252214E-12));
#9752=CARTESIAN_POINT('',(0.9,1.32024227787037,0.));
#9753=CARTESIAN_POINT('',(0.9,1.39290118819044,0.));
#9754=CARTESIAN_POINT('',(0.297857995688647,1.306435779838,0.));
#9755=CARTESIAN_POINT('Ctrl Pts',(0.9,1.32024227787037,-6.93889390390723E-18));
#9756=CARTESIAN_POINT('Ctrl Pts',(0.699470323836888,1.31560060380002,-4.72996299588896E-10));
#9757=CARTESIAN_POINT('Ctrl Pts',(0.498765843889866,1.3110112408976,-1.02277582142263E-13));
#9758=CARTESIAN_POINT('Ctrl Pts',(0.297857995688647,1.306435779838,-1.00157829096748E-16));
#9759=CARTESIAN_POINT('Ctrl Pts',(0.297857995688647,1.306435779838,-1.95156391047391E-17));
#9760=CARTESIAN_POINT('Ctrl Pts',(0.289922476296638,1.30625505685688,-1.46278605970555E-13));
#9761=CARTESIAN_POINT('Ctrl Pts',(0.282050301799808,1.30510306275878,-1.25203502999379E-6));
#9762=CARTESIAN_POINT('Ctrl Pts',(0.274405144964298,1.30305953674341,-1.39678564665046E-6));
#9763=CARTESIAN_POINT('Ctrl Pts',(0.269498922713003,1.30174811919849,-1.48967827287246E-6));
#9764=CARTESIAN_POINT('Ctrl Pts',(0.26468600784495,1.30006837070384,-1.17796618578504E-6));
#9765=CARTESIAN_POINT('Ctrl Pts',(0.260012701218123,1.29803054880949,-5.63923085528507E-7));
#9766=CARTESIAN_POINT('Ctrl Pts',(0.252740988282594,1.29485967708789,3.91534262267771E-7));
#9767=CARTESIAN_POINT('Ctrl Pts',(0.245891302634708,1.2908611961912,2.26944434681222E-6));
#9768=CARTESIAN_POINT('Ctrl Pts',(0.239629152465829,1.28609427281,1.73040332626933E-6));
#9769=CARTESIAN_POINT('Ctrl Pts',(0.238677421334952,1.28536978852616,1.6484790500646E-6));
#9770=CARTESIAN_POINT('Ctrl Pts',(0.23773930716971,1.28462746803483,1.50379952206709E-6));
#9771=CARTESIAN_POINT('Ctrl Pts',(0.236815449960777,1.28386742955246,1.27686598471174E-6));
#9772=CARTESIAN_POINT('Ctrl Pts',(0.233849259515119,1.28142720517261,5.48259784756267E-7));
#9773=CARTESIAN_POINT('Ctrl Pts',(0.231029859162728,1.27880446664625,-1.01231737317126E-6));
#9774=CARTESIAN_POINT('Ctrl Pts',(0.228365947504865,1.27601569667724,-2.73789903475208E-6));
#9775=CARTESIAN_POINT('Ctrl Pts',(0.222875659368053,1.2702680771449,-6.2943009513513E-6));
#9776=CARTESIAN_POINT('Ctrl Pts',(0.218108003769119,1.26388547870891,-1.02458913084139E-5));
#9777=CARTESIAN_POINT('Ctrl Pts',(0.214119068651703,1.25703104885628,-1.16727273233865E-5));
#9778=CARTESIAN_POINT('Ctrl Pts',(0.211608035823831,1.25271618840614,-1.25709199407453E-5));
#9779=CARTESIAN_POINT('Ctrl Pts',(0.209406266788438,1.24821342134138,-1.25531979180244E-5));
#9780=CARTESIAN_POINT('Ctrl Pts',(0.207536767894457,1.24355803714115,-1.16467700682383E-5));
#9781=CARTESIAN_POINT('Ctrl Pts',(0.204585779527196,1.23620955211972,-1.02159812889057E-5));
#9782=CARTESIAN_POINT('Ctrl Pts',(0.20249437279756,1.22856635796309,-6.44823334219156E-6));
#9783=CARTESIAN_POINT('Ctrl Pts',(0.201333199355162,1.22077498745768,-3.37414558979738E-6));
#9784=CARTESIAN_POINT('Ctrl Pts',(0.200635497716839,1.21609347152911,-1.5270519663277E-6));
#9785=CARTESIAN_POINT('Ctrl Pts',(0.200274469246579,1.21135795995708,-3.76748562593766E-12));
#9786=CARTESIAN_POINT('Ctrl Pts',(0.200274469199584,1.20659878095028,6.07153216591882E-18));
#9787=CARTESIAN_POINT('',(-2.81723893694256E-19,1.20714678905882,-2.77862675945125E-17));
#9788=CARTESIAN_POINT('',(0.,-1.5,0.));
#9789=CARTESIAN_POINT('',(0.292751161823634,1.50665779898694,0.));
#9790=CARTESIAN_POINT('Ctrl Pts',(0.292751161823634,1.50665779898694,-4.77048955893622E-17));
#9791=CARTESIAN_POINT('Ctrl Pts',(0.274916014309114,1.50625165707847,3.84528327419955E-12));
#9792=CARTESIAN_POINT('Ctrl Pts',(0.257184594685611,1.50420857033458,-2.03607170333744E-6));
#9793=CARTESIAN_POINT('Ctrl Pts',(0.239764500086274,1.50063675387888,-2.79213621391921E-6));
#9794=CARTESIAN_POINT('Ctrl Pts',(0.222116086584643,1.49701812291205,-3.55811018958082E-6));
#9795=CARTESIAN_POINT('Ctrl Pts',(0.204785660682177,1.49183000356027,-2.9511242418033E-6));
#9796=CARTESIAN_POINT('Ctrl Pts',(0.187998620502071,1.4851341555102,-6.80337370794577E-7));
#9797=CARTESIAN_POINT('Ctrl Pts',(0.185044527596802,1.48395585623842,-2.80736529130144E-7));
#9798=CARTESIAN_POINT('Ctrl Pts',(0.182107319868513,1.48273075079643,1.61255976403501E-7));
#9799=CARTESIAN_POINT('Ctrl Pts',(0.17918831289364,1.48145903083089,6.35063889779883E-7));
#9800=CARTESIAN_POINT('Ctrl Pts',(0.162608037952008,1.47423552404966,3.32634402063389E-6));
#9801=CARTESIAN_POINT('Ctrl Pts',(0.146760254055949,1.46557586252388,7.36741945499403E-6));
#9802=CARTESIAN_POINT('Ctrl Pts',(0.131860714325404,1.4555643673366,8.80872142158042E-6));
#9803=CARTESIAN_POINT('Ctrl Pts',(0.12416804976458,1.45039541073654,9.55286874158632E-6));
#9804=CARTESIAN_POINT('Ctrl Pts',(0.116728404005452,1.44486529627202,9.54902993357918E-6));
#9805=CARTESIAN_POINT('Ctrl Pts',(0.109574210210226,1.43898090192647,7.86258910610491E-6));
#9806=CARTESIAN_POINT('Ctrl Pts',(0.100675189791982,1.43166137062374,5.76484451217541E-6));
#9807=CARTESIAN_POINT('Ctrl Pts',(0.0922175942578585,1.42379373777092,1.07962821494929E-6));
#9808=CARTESIAN_POINT('Ctrl Pts',(0.0842272493232774,1.41542759110015,-4.17082519724513E-6));
#9809=CARTESIAN_POINT('Ctrl Pts',(0.0719003514327883,1.40252093480537,-1.22708263387205E-5));
#9810=CARTESIAN_POINT('Ctrl Pts',(0.0607923942774574,1.38854365509349,-2.1446290640466E-5));
#9811=CARTESIAN_POINT('Ctrl Pts',(0.0509667079859164,1.37370740939602,-2.73088451608079E-5));
#9812=CARTESIAN_POINT('Ctrl Pts',(0.040988527714452,1.35864090617899,-3.32623861267576E-5));
#9813=CARTESIAN_POINT('Ctrl Pts',(0.0323319291028794,1.34268723517955,-3.58272570146011E-5));
#9814=CARTESIAN_POINT('Ctrl Pts',(0.0251054147216294,1.32603775378173,-3.42048160832586E-5));
#9815=CARTESIAN_POINT('Ctrl Pts',(0.0239557673766072,1.32338903116455,-3.39467061825833E-5));
#9816=CARTESIAN_POINT('Ctrl Pts',(0.022842414085455,1.32072266145131,-3.35898145907185E-5));
#9817=CARTESIAN_POINT('Ctrl Pts',(0.0217659098422027,1.31803938112476,-3.31388957009043E-5));
#9818=CARTESIAN_POINT('Ctrl Pts',(0.0146851456525434,1.30038996137917,-3.01729526055095E-5));
#9819=CARTESIAN_POINT('Ctrl Pts',(0.00925910545076598,1.282173175788,-2.28911926108039E-5));
#9820=CARTESIAN_POINT('Ctrl Pts',(0.0055880418397064,1.26361786690427,-1.53360241296986E-5));
#9821=CARTESIAN_POINT('Ctrl Pts',(0.00217213684284492,1.24635225152695,
-8.30598038733772E-6));
#9822=CARTESIAN_POINT('Ctrl Pts',(0.000275638047107462,1.2287919996398,
-1.11502351997496E-6));
#9823=CARTESIAN_POINT('Ctrl Pts',(2.78020181985954E-5,1.21111091902543,
-1.13803743790751E-7));
#9824=CARTESIAN_POINT('Ctrl Pts',(9.289355304618E-6,1.20979019141994,-3.90154078055202E-8));
#9825=CARTESIAN_POINT('Ctrl Pts',(3.5054796412911E-11,1.20846879032832,
-2.82152417201308E-12));
#9826=CARTESIAN_POINT('Ctrl Pts',(6.5594231435373E-18,1.20714678905882,
2.42861286636753E-17));
#9827=CARTESIAN_POINT('',(12.8678148030684,2.16300527278356,0.));
#9828=CARTESIAN_POINT('Ctrl Pts',(0.292751161823634,1.50665779898694,0.));
#9829=CARTESIAN_POINT('Ctrl Pts',(4.48443904223854,1.60211086545473,0.));
#9830=CARTESIAN_POINT('Ctrl Pts',(8.67612692265345,1.70561506876628,0.));
#9831=CARTESIAN_POINT('Ctrl Pts',(12.8678148030684,2.16300527278356,0.));
#9832=CARTESIAN_POINT('',(13.2,1.86519007666192,1.29914761427265E-16));
#9833=CARTESIAN_POINT('Ctrl Pts',(13.2,1.86519007666192,1.40512601554121E-16));
#9834=CARTESIAN_POINT('Ctrl Pts',(13.2000000013352,1.88296731840607,9.35191444695304E-11));
#9835=CARTESIAN_POINT('Ctrl Pts',(13.1983511006715,1.90064589040826,-4.81925060583158E-6));
#9836=CARTESIAN_POINT('Ctrl Pts',(13.1951709302004,1.91804121845656,-9.22684518112407E-6));
#9837=CARTESIAN_POINT('Ctrl Pts',(13.1919252271695,1.93579500539423,-1.37252653764835E-5));
#9838=CARTESIAN_POINT('Ctrl Pts',(13.1870840836913,1.95325521073227,-1.77396479500911E-5));
#9839=CARTESIAN_POINT('Ctrl Pts',(13.1807207319279,1.9702167899609,-1.88895599539727E-5));
#9840=CARTESIAN_POINT('Ctrl Pts',(13.179605107926,1.97319049715201,-1.90911627380646E-5));
#9841=CARTESIAN_POINT('Ctrl Pts',(13.1784425783122,1.97614882406338,-1.92137058190342E-5));
#9842=CARTESIAN_POINT('Ctrl Pts',(13.1772333926356,1.97909058504493,-1.92562174744009E-5));
#9843=CARTESIAN_POINT('Ctrl Pts',(13.1703491364924,1.99583891121373,-1.94982490583826E-5));
#9844=CARTESIAN_POINT('Ctrl Pts',(13.1620175712498,2.0119031422279,-1.67925698753361E-5));
#9845=CARTESIAN_POINT('Ctrl Pts',(13.1523342210936,2.02708796667103,-1.30402710852334E-5));
#9846=CARTESIAN_POINT('Ctrl Pts',(13.1443502942575,2.03960786168842,-9.94649893779315E-6));
#9847=CARTESIAN_POINT('Ctrl Pts',(13.1354462980072,2.05153020544825,-6.18593217696112E-6));
#9848=CARTESIAN_POINT('Ctrl Pts',(13.1256528604983,2.06273196126272,-4.73977425690188E-6));
#9849=CARTESIAN_POINT('Ctrl Pts',(13.1217453950533,2.06720132901318,-4.16277439392992E-6));
#9850=CARTESIAN_POINT('Ctrl Pts',(13.1176961215346,2.07155579183536,-3.97575052791371E-6));
#9851=CARTESIAN_POINT('Ctrl Pts',(13.1135113749213,2.07579033931164,-3.99023031318383E-6));
#9852=CARTESIAN_POINT('Ctrl Pts',(13.1009362730034,2.08851509208914,-4.03374185458576E-6));
#9853=CARTESIAN_POINT('Ctrl Pts',(13.0872516297578,2.10004749226926,-5.60236028337187E-6));
#9854=CARTESIAN_POINT('Ctrl Pts',(13.0726646436523,2.11028882659185,-6.03124820804926E-6));
#9855=CARTESIAN_POINT('Ctrl Pts',(13.0580194031224,2.12057106059247,-6.46184893473862E-6));
#9856=CARTESIAN_POINT('Ctrl Pts',(13.0424632957183,2.12955278528135,-5.76500392338198E-6));
#9857=CARTESIAN_POINT('Ctrl Pts',(13.0261754841647,2.13709349482706,-4.98347139369932E-6));
#9858=CARTESIAN_POINT('Ctrl Pts',(13.0233759049672,2.13838960594114,-4.84914013593099E-6));
#9859=CARTESIAN_POINT('Ctrl Pts',(13.0205546633935,2.13964302898522,-4.72077764982159E-6));
#9860=CARTESIAN_POINT('Ctrl Pts',(13.0177126224567,2.14085289970554,-4.61407510358037E-6));
#9861=CARTESIAN_POINT('Ctrl Pts',(13.0148367726024,2.14207716304734,-4.50610322390289E-6));
#9862=CARTESIAN_POINT('Ctrl Pts',(13.0119432782921,2.14325527660784,-4.42172619954107E-6));
#9863=CARTESIAN_POINT('Ctrl Pts',(13.0090331608036,2.14438664763146,-4.38057543634576E-6));
#9864=CARTESIAN_POINT('Ctrl Pts',(12.9922536897216,2.1509100294015,-4.14330390220891E-6));
#9865=CARTESIAN_POINT('Ctrl Pts',(12.9749229882599,2.15588345271621,-5.05640020348117E-6));
#9866=CARTESIAN_POINT('Ctrl Pts',(12.9572550825995,2.15928949382789,-4.85686529648217E-6));
#9867=CARTESIAN_POINT('Ctrl Pts',(12.9529252316797,2.16012420794307,-4.80796553341985E-6));
#9868=CARTESIAN_POINT('Ctrl Pts',(12.9485750628159,2.16086455090717,-4.70814629363608E-6));
#9869=CARTESIAN_POINT('Ctrl Pts',(12.944207640703,2.16150979950679,-4.55317442353944E-6));
#9870=CARTESIAN_POINT('Ctrl Pts',(12.9263774359968,2.16414405704371,-3.92049452767182E-6));
#9871=CARTESIAN_POINT('Ctrl Pts',(12.9083632163621,2.16518216214944,-2.15504024707585E-6));
#9872=CARTESIAN_POINT('Ctrl Pts',(12.8903762705535,2.16459816844574,-9.12104093693782E-7));
#9873=CARTESIAN_POINT('Ctrl Pts',(12.8828459063217,2.16435367528137,-3.91739933400607E-7));
#9874=CARTESIAN_POINT('Ctrl Pts',(12.8753202361859,2.1638242536466,5.87463683432524E-12));
#9875=CARTESIAN_POINT('Ctrl Pts',(12.8678148030684,2.16300527278357,2.8796409701215E-16));
#9876=CARTESIAN_POINT('',(13.2,-1.86519007666192,1.11326398357188E-16));
#9877=CARTESIAN_POINT('',(13.2,2.2,0.));
#9878=CARTESIAN_POINT('',(12.8678148030684,-2.16300527278356,1.38777878078145E-17));
#9879=CARTESIAN_POINT('Ctrl Pts',(12.8678148030684,-2.16300527278357,2.56739074444567E-16));
#9880=CARTESIAN_POINT('Ctrl Pts',(12.8854929372559,-2.16493428409685,8.24591542686399E-11));
#9881=CARTESIAN_POINT('Ctrl Pts',(12.9032520674897,-2.16521372082443,-4.52295339524789E-6));
#9882=CARTESIAN_POINT('Ctrl Pts',(12.9208958607904,-2.1639404182545,-8.68231213275745E-6));
#9883=CARTESIAN_POINT('Ctrl Pts',(12.9389012534027,-2.16264102008682,-1.29269145154966E-5));
#9884=CARTESIAN_POINT('Ctrl Pts',(12.9567880250381,-2.15972433317902,-1.67278855193166E-5));
#9885=CARTESIAN_POINT('Ctrl Pts',(12.9743443410528,-2.15524079327399,-1.78237954457702E-5));
#9886=CARTESIAN_POINT('Ctrl Pts',(12.9774431846623,-2.15444940919484,-1.80172331504298E-5));
#9887=CARTESIAN_POINT('Ctrl Pts',(12.9805316913262,-2.15360908525727,-1.81351031595367E-5));
#9888=CARTESIAN_POINT('Ctrl Pts',(12.9836086301392,-2.15271994254544,-1.81766625580856E-5));
#9889=CARTESIAN_POINT('Ctrl Pts',(13.0010041030966,-2.14769317440371,-1.84116186093898E-5));
#9890=CARTESIAN_POINT('Ctrl Pts',(13.017876958431,-2.14115457229109,-1.5854618169158E-5));
#9891=CARTESIAN_POINT('Ctrl Pts',(13.0340226638693,-2.13317744288338,-1.23136839993165E-5));
#9892=CARTESIAN_POINT('Ctrl Pts',(13.0473215411186,-2.12660684953271,-9.39709115965876E-6));
#9893=CARTESIAN_POINT('Ctrl Pts',(13.060127470267,-2.11905920305061,-5.85016632862467E-6));
#9894=CARTESIAN_POINT('Ctrl Pts',(13.0723151314263,-2.11055132433008,-4.53327195050794E-6));
#9895=CARTESIAN_POINT('Ctrl Pts',(13.0772147086919,-2.10713106111368,-4.00386555564548E-6));
#9896=CARTESIAN_POINT('Ctrl Pts',(13.0820141951123,-2.10355537352593,-3.85636210984559E-6));
#9897=CARTESIAN_POINT('Ctrl Pts',(13.0867078006727,-2.0998301147952,-3.90248451975241E-6));
#9898=CARTESIAN_POINT('Ctrl Pts',(13.1007249787291,-2.08870484782034,-4.04022639510273E-6));
#9899=CARTESIAN_POINT('Ctrl Pts',(13.1136765748478,-2.07634683247102,-5.5945154994439E-6));
#9900=CARTESIAN_POINT('Ctrl Pts',(13.1254414850725,-2.06295113861397,-5.97495381195624E-6));
#9901=CARTESIAN_POINT('Ctrl Pts',(13.1372476314214,-2.04950849272046,-6.35672556443159E-6));
#9902=CARTESIAN_POINT('Ctrl Pts',(13.1478597809499,-2.03501968083851,-5.56609061204695E-6));
#9903=CARTESIAN_POINT('Ctrl Pts',(13.1571184147632,-2.01964723728874,-4.75455255839871E-6));
#9904=CARTESIAN_POINT('Ctrl Pts',(13.158708901902,-2.01700649414547,-4.61514313115074E-6));
#9905=CARTESIAN_POINT('Ctrl Pts',(13.1602593369672,-2.01433961799121,-4.48389992381974E-6));
#9906=CARTESIAN_POINT('Ctrl Pts',(13.1617687665475,-2.01164737048868,-4.37752847101542E-6));
#9907=CARTESIAN_POINT('Ctrl Pts',(13.1632768494098,-2.00895752501823,-4.27125192317111E-6));
#9908=CARTESIAN_POINT('Ctrl Pts',(13.164742106841,-2.00624572954308,-4.19089851494128E-6));
#9909=CARTESIAN_POINT('Ctrl Pts',(13.1661638648313,-2.00351289682408,-4.15637526360595E-6));
#9910=CARTESIAN_POINT('Ctrl Pts',(13.1744716670281,-1.98754405133797,-3.95464448717833E-6));
#9911=CARTESIAN_POINT('Ctrl Pts',(13.181298057795,-1.97085874357403,-5.01850453361653E-6));
#9912=CARTESIAN_POINT('Ctrl Pts',(13.1866022393826,-1.95366776591112,-4.89891140766866E-6));
#9913=CARTESIAN_POINT('Ctrl Pts',(13.1879075264936,-1.94943729958961,-4.86948116225E-6));
#9914=CARTESIAN_POINT('Ctrl Pts',(13.1891204013114,-1.94517611908519,-4.78523710928743E-6));
#9915=CARTESIAN_POINT('Ctrl Pts',(13.1902397948733,-1.94088722910442,-4.64104147683466E-6));
#9916=CARTESIAN_POINT('Ctrl Pts',(13.1947901580114,-1.92345278286841,-4.05488258426869E-6));
#9917=CARTESIAN_POINT('Ctrl Pts',(13.1977733658442,-1.90566244769967,-2.24449026644408E-6));
#9918=CARTESIAN_POINT('Ctrl Pts',(13.1991406030032,-1.88772335428786,-9.50757284845071E-7));
#9919=CARTESIAN_POINT('Ctrl Pts',(13.1997114533543,-1.8802334044254,-4.10596478211383E-7));
#9920=CARTESIAN_POINT('Ctrl Pts',(13.2000000000958,-1.87271737110067,6.9401096738129E-12));
#9921=CARTESIAN_POINT('Ctrl Pts',(13.2,-1.86519007666192,1.81278603239576E-16));
#9922=CARTESIAN_POINT('',(0.292751161823634,-1.50665779898694,-1.38777878078145E-17));
#9923=CARTESIAN_POINT('Ctrl Pts',(12.8678148030684,-2.16300527278356,0.));
#9924=CARTESIAN_POINT('Ctrl Pts',(8.67612692265345,-1.70561506876628,0.));
#9925=CARTESIAN_POINT('Ctrl Pts',(4.48443904223854,-1.60211086545473,0.));
#9926=CARTESIAN_POINT('Ctrl Pts',(0.292751161823634,-1.50665779898694,0.));
#9927=CARTESIAN_POINT('',(4.02814324098787E-18,-1.20714678905882,5.54818711994559E-17));
#9928=CARTESIAN_POINT('Ctrl Pts',(-2.22044604925031E-16,-1.20714678905882,
-3.98986399474666E-17));
#9929=CARTESIAN_POINT('Ctrl Pts',(2.12382277713531E-10,-1.2249878157372,
-1.35440422383976E-12));
#9930=CARTESIAN_POINT('Ctrl Pts',(0.00163882612763064,-1.24276245549475,
-1.96699749426327E-6));
#9931=CARTESIAN_POINT('Ctrl Pts',(0.00481304415265273,-1.26026068126938,
-2.66007142975038E-6));
#9932=CARTESIAN_POINT('Ctrl Pts',(0.00802873944670128,-1.27798755504872,
-3.36220171040687E-6));
#9933=CARTESIAN_POINT('Ctrl Pts',(0.0128206026099745,-1.29543230475431,
-2.69550948014298E-6));
#9934=CARTESIAN_POINT('Ctrl Pts',(0.0191320595672371,-1.31236817798419,
-4.00401478067381E-7));
#9935=CARTESIAN_POINT('Ctrl Pts',(0.0202443702650641,-1.31535290133701,
4.0809101773195E-9));
#9936=CARTESIAN_POINT('Ctrl Pts',(0.0214039964883031,-1.3183217636574,4.5005107558061E-7));
#9937=CARTESIAN_POINT('Ctrl Pts',(0.0226107760969305,-1.32127343934773,
9.26779280916758E-7));
#9938=CARTESIAN_POINT('Ctrl Pts',(0.0294548697216842,-1.33801348419941,
3.63048130534217E-6));
#9939=CARTESIAN_POINT('Ctrl Pts',(0.0377511831708778,-1.35405403406083,
7.64722139837078E-6));
#9940=CARTESIAN_POINT('Ctrl Pts',(0.0474204318104353,-1.36917746582299,
9.03443059383348E-6));
#9941=CARTESIAN_POINT('Ctrl Pts',(0.0524109755304394,-1.37698305136733,
9.75040433665629E-6));
#9942=CARTESIAN_POINT('Ctrl Pts',(0.0577680562174045,-1.38454410063597,
9.71159147480002E-6));
#9943=CARTESIAN_POINT('Ctrl Pts',(0.0634855547170043,-1.39182806229354,
7.98761394269614E-6));
#9944=CARTESIAN_POINT('Ctrl Pts',(0.0706048733905122,-1.40089791062835,
5.84095042579577E-6));
#9945=CARTESIAN_POINT('Ctrl Pts',(0.0782829434694699,-1.40953838460506,
1.09773645972912E-6));
#9946=CARTESIAN_POINT('Ctrl Pts',(0.0864706998703675,-1.41772246232928,
-4.21049985396393E-6));
#9947=CARTESIAN_POINT('Ctrl Pts',(0.0990944981487371,-1.43034058886193,
-1.2394683793612E-5));
#9948=CARTESIAN_POINT('Ctrl Pts',(0.112816484288725,-1.44176429483685,-2.16481703631134E-5));
#9949=CARTESIAN_POINT('Ctrl Pts',(0.127426518150943,-1.45192534842919,-2.7562374581111E-5));
#9950=CARTESIAN_POINT('Ctrl Pts',(0.142261949549145,-1.46224316253723,-3.35678206860622E-5));
#9951=CARTESIAN_POINT('Ctrl Pts',(0.158014355623482,-1.47125989363127,-3.6155642403295E-5));
#9952=CARTESIAN_POINT('Ctrl Pts',(0.17449494651519,-1.47886261331763,-3.45187637154371E-5));
#9953=CARTESIAN_POINT('Ctrl Pts',(0.177115379630184,-1.48007145458801,-3.42584981007467E-5));
#9954=CARTESIAN_POINT('Ctrl Pts',(0.179754261386328,-1.48124444832217,-3.38986806574493E-5));
#9955=CARTESIAN_POINT('Ctrl Pts',(0.18241086941249,-1.48238102342202,-3.34441145409493E-5));
#9956=CARTESIAN_POINT('Ctrl Pts',(0.199890279181845,-1.48985922935543,-3.04532527580594E-5));
#9957=CARTESIAN_POINT('Ctrl Pts',(0.217974246898519,-1.49569663469242,-2.31073027206853E-5));
#9958=CARTESIAN_POINT('Ctrl Pts',(0.236436446036386,-1.49978781870256,-1.54828395726751E-5));
#9959=CARTESIAN_POINT('Ctrl Pts',(0.253618559172887,-1.50359533838099,-8.38702246898572E-6));
#9960=CARTESIAN_POINT('Ctrl Pts',(0.271129804961754,-1.50589051664322,-1.1237837803371E-6));
#9961=CARTESIAN_POINT('Ctrl Pts',(0.288799387895208,-1.50654014509364,-1.14426782679271E-7));
#9962=CARTESIAN_POINT('Ctrl Pts',(0.290115790923368,-1.5065885431154,-3.92285953074499E-8));
#9963=CARTESIAN_POINT('Ctrl Pts',(0.291433072638222,-1.50662778343727,-2.32210426557352E-12));
#9964=CARTESIAN_POINT('Ctrl Pts',(0.292751161823634,-1.50665779898694,2.86229373536173E-17));
#9965=CARTESIAN_POINT('',(0.,-1.5,0.));
#9966=CARTESIAN_POINT('',(0.297857995688647,-1.306435779838,0.));
#9967=CARTESIAN_POINT('Ctrl Pts',(0.200274469199585,-1.20659878095028,-5.63785129692462E-18));
#9968=CARTESIAN_POINT('Ctrl Pts',(0.200274469233139,-1.21453676310593,-8.71436967499621E-13));
#9969=CARTESIAN_POINT('Ctrl Pts',(0.201246859971722,-1.22243356087926,-1.21395871814677E-6));
#9970=CARTESIAN_POINT('Ctrl Pts',(0.203115675186186,-1.23012372049816,-1.3343733317444E-6));
#9971=CARTESIAN_POINT('Ctrl Pts',(0.204315340901654,-1.23506033529553,-1.41167219064517E-6));
#9972=CARTESIAN_POINT('Ctrl Pts',(0.20588557457721,-1.23991201018842,-1.08820351238587E-6));
#9973=CARTESIAN_POINT('Ctrl Pts',(0.207817175189242,-1.24463217458037,-4.7123943162984E-7));
#9974=CARTESIAN_POINT('Ctrl Pts',(0.210821635148072,-1.25197403646754,4.8840194822981E-7));
#9975=CARTESIAN_POINT('Ctrl Pts',(0.214662962735955,-1.25891288736431,2.34840446672759E-6));
#9976=CARTESIAN_POINT('Ctrl Pts',(0.219285851586231,-1.26528190572196,1.77850405974346E-6));
#9977=CARTESIAN_POINT('Ctrl Pts',(0.219987799701267,-1.26624898941694,1.69196931287913E-6));
#9978=CARTESIAN_POINT('Ctrl Pts',(0.220707854727247,-1.26720289123473,1.54254180957111E-6));
#9979=CARTESIAN_POINT('Ctrl Pts',(0.221445913570039,-1.26814297034805,1.31084431541716E-6));
#9980=CARTESIAN_POINT('Ctrl Pts',(0.223819423285066,-1.27116615329633,5.65732650279818E-7));
#9981=CARTESIAN_POINT('Ctrl Pts',(0.226378993511503,-1.27404655624932,-1.0141799309673E-6));
#9982=CARTESIAN_POINT('Ctrl Pts',(0.229108317341547,-1.27677508245113,-2.75886047820546E-6));
#9983=CARTESIAN_POINT('Ctrl Pts',(0.234729699316268,-1.28239482161129,-6.35224711555937E-6));
#9984=CARTESIAN_POINT('Ctrl Pts',(0.241002345945823,-1.28730653457646,-1.03364935932408E-5));
#9985=CARTESIAN_POINT('Ctrl Pts',(0.247764463424355,-1.29145035967733,-1.17765252099068E-5));
#9986=CARTESIAN_POINT('Ctrl Pts',(0.25202072563572,-1.29405859685204,-1.26829206064147E-5));
#9987=CARTESIAN_POINT('Ctrl Pts',(0.25647185453211,-1.29636195369988,-1.26655904667795E-5));
#9988=CARTESIAN_POINT('Ctrl Pts',(0.261083107941716,-1.29833661269995,-1.17517412599227E-5));
#9989=CARTESIAN_POINT('Ctrl Pts',(0.268362152520619,-1.30145368947124,-1.0309194402435E-5));
#9990=CARTESIAN_POINT('Ctrl Pts',(0.275955349537693,-1.30371808689536,-6.50743389458559E-6));
#9991=CARTESIAN_POINT('Ctrl Pts',(0.283717840216357,-1.30505580179168,-3.40467605837577E-6));
#9992=CARTESIAN_POINT('Ctrl Pts',(0.288379557365255,-1.3058591584372,-1.54133347766382E-6));
#9993=CARTESIAN_POINT('Ctrl Pts',(0.293102847896135,-1.30632748638856,-3.09915230996644E-12));
#9994=CARTESIAN_POINT('Ctrl Pts',(0.297857995688647,-1.306435779838,2.90566182226115E-17));
#9995=CARTESIAN_POINT('',(0.9,-1.32024227787037,0.));
#9996=CARTESIAN_POINT('Ctrl Pts',(0.297857995688651,-1.306435779838,-5.81335652359571E-17));
#9997=CARTESIAN_POINT('Ctrl Pts',(0.498765834064439,-1.31101124067384,-1.02216845336465E-13));
#9998=CARTESIAN_POINT('Ctrl Pts',(0.699470314209512,-1.31560060357718,-4.73070532165219E-10));
#9999=CARTESIAN_POINT('Ctrl Pts',(0.9,-1.32024227787037,4.62320796019307E-17));
#10000=CARTESIAN_POINT('',(0.9,1.39290118819044,0.));
#10001=CARTESIAN_POINT('',(4.3,-1.41116952203211,0.));
#10002=CARTESIAN_POINT('Ctrl Pts',(1.10000000020724,-1.32489175811528,-9.82782277325449E-12));
#10003=CARTESIAN_POINT('Ctrl Pts',(2.16992692797068,-1.34987955410658,4.63225598025733E-9));
#10004=CARTESIAN_POINT('Ctrl Pts',(3.23514201430925,-1.37672428034078,3.20747301048384E-8));
#10005=CARTESIAN_POINT('Ctrl Pts',(4.3,-1.41116952203211,-8.74629427996717E-16));
#10006=CARTESIAN_POINT('',(4.3,1.48481481481482,0.));
#10007=CARTESIAN_POINT('',(8.7,-1.61160179736194,0.));
#10008=CARTESIAN_POINT('Ctrl Pts',(4.50000000001737,-1.41772989873549,-1.00870158580013E-12));
#10009=CARTESIAN_POINT('Ctrl Pts',(5.14541122039116,-1.43919849219739,1.84287460122322E-8));
#10010=CARTESIAN_POINT('Ctrl Pts',(5.79079200637672,-1.46358894290692,-2.29215846350395E-9));
#10011=CARTESIAN_POINT('Ctrl Pts',(6.43711407552466,-1.49221504703413,-7.12038357450289E-9));
#10012=CARTESIAN_POINT('Ctrl Pts',(6.48784335049204,-1.49446188584227,-7.49934689782436E-9));
#10013=CARTESIAN_POINT('Ctrl Pts',(6.5385784252675,-1.49673484630497,-7.6873350528488E-9));
#10014=CARTESIAN_POINT('Ctrl Pts',(6.58931977021612,-1.49903457911226,-7.60400982311631E-9));
#10015=CARTESIAN_POINT('Ctrl Pts',(7.29382172663923,-1.5309644828944,-6.44710735180711E-9));
#10016=CARTESIAN_POINT('Ctrl Pts',(7.99729122590638,-1.56795478022256,5.29179522587699E-9));
#10017=CARTESIAN_POINT('Ctrl Pts',(8.70000000002062,-1.61160179731554,-3.21479112539667E-13));
#10018=CARTESIAN_POINT('',(8.7,1.68851851851852,0.));
#10019=CARTESIAN_POINT('',(12.6,-1.93292824674167,0.));
#10020=CARTESIAN_POINT('',(12.8889963716306,-1.96391015057091,0.));
#10021=CARTESIAN_POINT('Ctrl Pts',(12.6000000004653,-1.93292824679067,-1.00288700954909E-16));
#10022=CARTESIAN_POINT('Ctrl Pts',(12.6963367945484,-1.94307238002033,2.28133307867826E-10));
#10023=CARTESIAN_POINT('Ctrl Pts',(12.7926686848896,-1.9533982851754,-5.07154825701885E-13));
#10024=CARTESIAN_POINT('Ctrl Pts',(12.8889963716306,-1.96391015057091,2.24786696790336E-16));
#10025=CARTESIAN_POINT('',(12.9997255308004,-1.86463850151065,-1.38777878078145E-17));
#10026=CARTESIAN_POINT('Ctrl Pts',(12.8889963716306,-1.96391015057091,5.29090660172926E-17));
#10027=CARTESIAN_POINT('Ctrl Pts',(12.8968843421745,-1.96477093437063,1.28387508960266E-11));
#10028=CARTESIAN_POINT('Ctrl Pts',(12.9048206871516,-1.96464841285931,-2.5989605143924E-6));
#10029=CARTESIAN_POINT('Ctrl Pts',(12.9126487282508,-1.9636130141884,-4.24292438262167E-6));
#10030=CARTESIAN_POINT('Ctrl Pts',(12.9176900487482,-1.96294620923983,-5.30165014054907E-6));
#10031=CARTESIAN_POINT('Ctrl Pts',(12.9226867577298,-1.96189962975099,-6.00943773338864E-6));
#10032=CARTESIAN_POINT('Ctrl Pts',(12.9275953864907,-1.96048085896027,-6.09358828708331E-6));
#10033=CARTESIAN_POINT('Ctrl Pts',(12.9352257743335,-1.95827540160737,-6.22439902734509E-6));
#10034=CARTESIAN_POINT('Ctrl Pts',(12.9425549137553,-1.95519874430406,-4.64402662178521E-6));
#10035=CARTESIAN_POINT('Ctrl Pts',(12.949425376669,-1.9513005478593,-3.15156624759025E-6));
#10036=CARTESIAN_POINT('Ctrl Pts',(12.9520760960011,-1.94979656991686,-2.57575445499556E-6));
#10037=CARTESIAN_POINT('Ctrl Pts',(12.9546583803074,-1.94816978416017,-2.04880625960079E-6));
#10038=CARTESIAN_POINT('Ctrl Pts',(12.9571622133441,-1.9464211898676,-1.82278374303809E-6));
#10039=CARTESIAN_POINT('Ctrl Pts',(12.9587955877505,-1.9452804951316,-1.67533805140214E-6));
#10040=CARTESIAN_POINT('Ctrl Pts',(12.9603955609302,-1.94408794089591,-1.65796127395168E-6));
#10041=CARTESIAN_POINT('Ctrl Pts',(12.9619602112942,-1.94284549575182,-1.70649031798611E-6));
#10042=CARTESIAN_POINT('Ctrl Pts',(12.9681665721336,-1.93791719798967,-1.89898620422551E-6));
#10043=CARTESIAN_POINT('Ctrl Pts',(12.9737470546445,-1.93226498850035,-2.8025064238469E-6));
#10044=CARTESIAN_POINT('Ctrl Pts',(12.9786034821464,-1.926037248212,-2.79230211737029E-6));
#10045=CARTESIAN_POINT('Ctrl Pts',(12.9817011960737,-1.92206483066456,-2.78579321297956E-6));
#10046=CARTESIAN_POINT('Ctrl Pts',(12.9845038017717,-1.91785723501915,-2.48811564693169E-6));
#10047=CARTESIAN_POINT('Ctrl Pts',(12.9869771252785,-1.91344616543364,-2.2918341012218E-6));
#10048=CARTESIAN_POINT('Ctrl Pts',(12.9874796596041,-1.91254991636901,-2.25195326317628E-6));
#10049=CARTESIAN_POINT('Ctrl Pts',(12.9879679417815,-1.9116463809131,-2.21866365029432E-6));
#10050=CARTESIAN_POINT('Ctrl Pts',(12.98844174868,-1.91073586520696,-2.19841011183313E-6));
#10051=CARTESIAN_POINT('Ctrl Pts',(12.9918929665356,-1.9041036526468,-2.05088297829219E-6));
#10052=CARTESIAN_POINT('Ctrl Pts',(12.9945793344589,-1.89710244289626,-2.35789128083535E-6));
#10053=CARTESIAN_POINT('Ctrl Pts',(12.9964698429198,-1.88986530397042,-1.93853625224654E-6));
#10054=CARTESIAN_POINT('Ctrl Pts',(12.9984668213505,-1.88222058265133,-1.49556391743615E-6));
#10055=CARTESIAN_POINT('Ctrl Pts',(12.9995610814633,-1.87437060764114,-2.4459616079733E-7));
#10056=CARTESIAN_POINT('Ctrl Pts',(12.9997084424383,-1.86646992060833,-2.60951667192209E-8));
#10057=CARTESIAN_POINT('Ctrl Pts',(12.9997198235207,-1.86585972940924,-9.21975031242219E-9));
#10058=CARTESIAN_POINT('Ctrl Pts',(12.9997255308031,-1.86524923282631,2.14479566203628E-13));
#10059=CARTESIAN_POINT('Ctrl Pts',(12.9997255308004,-1.86463850151065,-9.54097911787244E-18));
#10060=CARTESIAN_POINT('',(12.9997255308004,1.86463850151064,1.38777878078145E-17));
#10061=CARTESIAN_POINT('',(12.9997255308004,1.1,0.));
#10062=CARTESIAN_POINT('',(12.8889963716306,1.96391015057091,0.));
#10063=CARTESIAN_POINT('Ctrl Pts',(12.9997255308004,1.86463850151065,-9.97465998686664E-18));
#10064=CARTESIAN_POINT('Ctrl Pts',(12.9997255309996,1.87257112921612,1.42345874390777E-11));
#10065=CARTESIAN_POINT('Ctrl Pts',(12.9987425107347,1.88044501776258,-2.76622459581243E-6));
#10066=CARTESIAN_POINT('Ctrl Pts',(12.9968635501128,1.8881121101061,-4.50602169498049E-6));
#10067=CARTESIAN_POINT('Ctrl Pts',(12.9956551765012,1.89304287446485,-5.62489820561454E-6));
#10068=CARTESIAN_POINT('Ctrl Pts',(12.994075066483,1.89788828888188,-6.37205869803057E-6));
#10069=CARTESIAN_POINT('Ctrl Pts',(12.9921354490207,1.90260616696402,-6.45954116508302E-6));
#10070=CARTESIAN_POINT('Ctrl Pts',(12.9891151690915,1.90995262200289,-6.59576469602218E-6));
#10071=CARTESIAN_POINT('Ctrl Pts',(12.9852608829945,1.91690476599405,-4.92589918404109E-6));
#10072=CARTESIAN_POINT('Ctrl Pts',(12.9806393828366,1.92331154882078,-3.3382766296878E-6));
#10073=CARTESIAN_POINT('Ctrl Pts',(12.9788533632605,1.92578750666072,-2.72472586378502E-6));
#10074=CARTESIAN_POINT('Ctrl Pts',(12.9769522584487,1.92818179997524,-2.1610482659023E-6));
#10075=CARTESIAN_POINT('Ctrl Pts',(12.9749381758772,1.93048453804291,-1.90960564360578E-6));
#10076=CARTESIAN_POINT('Ctrl Pts',(12.9736352090466,1.93197424425657,-1.74694031832382E-6));
#10077=CARTESIAN_POINT('Ctrl Pts',(12.9722849384098,1.93342561524533,-1.71698229815602E-6));
#10078=CARTESIAN_POINT('Ctrl Pts',(12.9708894910408,1.9348369915754,-1.75552529092739E-6));
#10079=CARTESIAN_POINT('Ctrl Pts',(12.9653179015399,1.94047218048862,-1.90941553332435E-6));
#10080=CARTESIAN_POINT('Ctrl Pts',(12.9590944588136,1.94540670303376,-2.83773366290493E-6));
#10081=CARTESIAN_POINT('Ctrl Pts',(12.9523775255978,1.94955941520082,-2.8574013135715E-6));
#10082=CARTESIAN_POINT('Ctrl Pts',(12.9480923984168,1.95220867479748,-2.86994846593266E-6));
#10083=CARTESIAN_POINT('Ctrl Pts',(12.9436054681019,1.95453912223498,-2.59559485065602E-6));
#10084=CARTESIAN_POINT('Ctrl Pts',(12.9389519978263,1.95652032281755,-2.39773084743613E-6));
#10085=CARTESIAN_POINT('Ctrl Pts',(12.9379934875219,1.95692840561619,-2.35697530915642E-6));
#10086=CARTESIAN_POINT('Ctrl Pts',(12.9370291206935,1.95732112306527,-2.32193094846859E-6));
#10087=CARTESIAN_POINT('Ctrl Pts',(12.9360592398442,1.95769827921557,-2.29894501965994E-6));
#10088=CARTESIAN_POINT('Ctrl Pts',(12.929096105975,1.96040602292032,-2.13392052256244E-6));
#10089=CARTESIAN_POINT('Ctrl Pts',(12.9218497638689,1.96231496375013,-2.36509085467933E-6));
#10090=CARTESIAN_POINT('Ctrl Pts',(12.9144555496645,1.96340894166242,-1.92146179377921E-6));
#10091=CARTESIAN_POINT('Ctrl Pts',(12.9066371708262,1.96456567495722,-1.45238421961943E-6));
#10092=CARTESIAN_POINT('Ctrl Pts',(12.8987125532455,1.96480297730229,-2.37321368026999E-7));
#10093=CARTESIAN_POINT('Ctrl Pts',(12.8908401755085,1.96409377829808,-2.55627471131237E-8));
#10094=CARTESIAN_POINT('Ctrl Pts',(12.89022523009,1.96403837970149,-9.02136684357828E-9));
#10095=CARTESIAN_POINT('Ctrl Pts',(12.8896106033158,1.96397717928728,1.9621770460073E-13));
#10096=CARTESIAN_POINT('Ctrl Pts',(12.8889963716306,1.96391015057091,-3.29597460435593E-17));
#10097=CARTESIAN_POINT('',(12.6,1.93292824674167,0.));
#10098=CARTESIAN_POINT('Ctrl Pts',(12.8889963716306,1.96391015057091,8.95144418658345E-17));
#10099=CARTESIAN_POINT('Ctrl Pts',(12.7926686852738,1.95339828521733,-5.07275478770449E-13));
#10100=CARTESIAN_POINT('Ctrl Pts',(12.6963367949308,1.94307238006059,2.28132759158623E-10));
#10101=CARTESIAN_POINT('Ctrl Pts',(12.6000000004652,1.93292824679066,-1.5019386425618E-16));
#10102=CARTESIAN_POINT('',(12.6,-1.99376954809806,0.));
#10103=CARTESIAN_POINT('Origin',(11.2,0.,0.));
#10104=CARTESIAN_POINT('',(10.8,-4.89858719658942E-17,0.7));
#10105=CARTESIAN_POINT('Origin',(11.2,0.,0.7));
#10106=CARTESIAN_POINT('',(10.8,-4.89858719658942E-17,0.));
#10107=CARTESIAN_POINT('Origin',(2.,0.,0.));
#10108=CARTESIAN_POINT('',(1.6,-4.89858719658941E-17,0.));
#10109=CARTESIAN_POINT('Origin',(12.6,-1.99376954809806,0.));
#10110=CARTESIAN_POINT('',(12.6,-1.90428042248893,0.60470250816874));
#10111=CARTESIAN_POINT('Ctrl Pts',(12.6,-1.93292824674167,0.));
#10112=CARTESIAN_POINT('Ctrl Pts',(12.6,-1.92814118331811,0.100975624959503));
#10113=CARTESIAN_POINT('Ctrl Pts',(12.6,-1.9233557423333,0.20195205683881));
#10114=CARTESIAN_POINT('Ctrl Pts',(12.6,-1.91380649287245,0.40351907263528));
#10115=CARTESIAN_POINT('Ctrl Pts',(12.6,-1.90904260275794,0.504111110768618));
#10116=CARTESIAN_POINT('Ctrl Pts',(12.6,-1.90428042248893,0.60470250816874));
#10117=CARTESIAN_POINT('',(12.6,1.90428042248893,0.60470250816874));
#10118=CARTESIAN_POINT('Ctrl Pts',(12.6,1.90428042248893,0.60470250816874));
#10119=CARTESIAN_POINT('Ctrl Pts',(12.6,1.90904310126474,0.504100580823831));
#10120=CARTESIAN_POINT('Ctrl Pts',(12.6,1.91380749024866,0.403498012513773));
#10121=CARTESIAN_POINT('Ctrl Pts',(12.6,1.92335674041114,0.201930996640285));
#10122=CARTESIAN_POINT('Ctrl Pts',(12.6,1.92814168252712,0.100965094925255));
#10123=CARTESIAN_POINT('Ctrl Pts',(12.6,1.93292824674167,0.));
#10124=CARTESIAN_POINT('',(12.6,1.80383022254432,0.7));
#10125=CARTESIAN_POINT('Ctrl Pts',(12.6,1.80383022254432,0.7));
#10126=CARTESIAN_POINT('Ctrl Pts',(12.6,1.81177675668304,0.7));
#10127=CARTESIAN_POINT('Ctrl Pts',(12.6000021803669,1.81966206665253,0.699006623620781));
#10128=CARTESIAN_POINT('Ctrl Pts',(12.6000040789681,1.8273451885609,0.69711902809518));
#10129=CARTESIAN_POINT('Ctrl Pts',(12.6000050614635,1.8313210797205,0.696142227980247));
#10130=CARTESIAN_POINT('Ctrl Pts',(12.6000059683507,1.83524283435206,0.694925046992878));
#10131=CARTESIAN_POINT('Ctrl Pts',(12.6000066021136,1.83908960013903,0.693475985595303));
#10132=CARTESIAN_POINT('Ctrl Pts',(12.6000078338507,1.84656590463324,0.690659691378536));
#10133=CARTESIAN_POINT('Ctrl Pts',(12.6000078244032,1.85367932786264,0.687000939374075));
#10134=CARTESIAN_POINT('Ctrl Pts',(12.6000065509639,1.86028396908448,0.682580904467878));
#10135=CARTESIAN_POINT('Ctrl Pts',(12.600005740321,1.86448833536622,0.679767209507086));
#10136=CARTESIAN_POINT('Ctrl Pts',(12.6000044390918,1.86848632867783,0.676643963831362));
#10137=CARTESIAN_POINT('Ctrl Pts',(12.6000033339006,1.8722338275817,0.673223162566374));
#10138=CARTESIAN_POINT('Ctrl Pts',(12.6000024442799,1.87525036668517,0.670469597843409));
#10139=CARTESIAN_POINT('Ctrl Pts',(12.600001679327,1.8780865799519,0.667539409933064));
#10140=CARTESIAN_POINT('Ctrl Pts',(12.600001676908,1.88072259809992,0.664442334323256));
#10141=CARTESIAN_POINT('Ctrl Pts',(12.6000016722164,1.88583495965423,0.658435786041233));
#10142=CARTESIAN_POINT('Ctrl Pts',(12.6000042182276,1.89019731592974,0.651802923597933));
#10143=CARTESIAN_POINT('Ctrl Pts',(12.6000050838539,1.89374834224248,0.644708005294394));
#10144=CARTESIAN_POINT('Ctrl Pts',(12.60000518898,1.89417959722901,0.643846361750254));
#10145=CARTESIAN_POINT('Ctrl Pts',(12.6000052753339,1.8945988291305,0.642977876839351));
#10146=CARTESIAN_POINT('Ctrl Pts',(12.6000053405091,1.89500587920016,0.642102827114796));
#10147=CARTESIAN_POINT('Ctrl Pts',(12.6000058761205,1.89835102950234,0.634911640898031));
#10148=CARTESIAN_POINT('Ctrl Pts',(12.6000044960414,1.90083797337412,0.627363460372113));
#10149=CARTESIAN_POINT('Ctrl Pts',(12.6000025707297,1.90241244660326,0.619625605651968));
#10150=CARTESIAN_POINT('Ctrl Pts',(12.6000013488022,1.90341170938816,0.614714661398562));
#10151=CARTESIAN_POINT('Ctrl Pts',(12.5999999979477,1.90404256918024,0.609726685483646));
#10152=CARTESIAN_POINT('Ctrl Pts',(12.6000000000242,1.90428042250026,0.604702508168697));
#10153=CARTESIAN_POINT('',(12.6,-1.8038302225439,0.7));
#10154=CARTESIAN_POINT('',(12.6,-0.996884774049031,0.7));
#10155=CARTESIAN_POINT('Ctrl Pts',(12.6000000000242,-1.90428042250026,0.604702508168697));
#10156=CARTESIAN_POINT('Ctrl Pts',(12.5999999967566,-1.90390613686288,0.612608546261599));
#10157=CARTESIAN_POINT('Ctrl Pts',(12.6000030637542,-1.90256112855112,0.620429349781532));
#10158=CARTESIAN_POINT('Ctrl Pts',(12.6000044618611,-1.90032851942705,0.628004813168584));
#10159=CARTESIAN_POINT('Ctrl Pts',(12.6000051410147,-1.89924399238468,0.63168472059761));
#10160=CARTESIAN_POINT('Ctrl Pts',(12.6000055125137,-1.89794920179963,0.635306724151721));
#10161=CARTESIAN_POINT('Ctrl Pts',(12.6000054780251,-1.8964494555225,0.638851301608537));
#10162=CARTESIAN_POINT('Ctrl Pts',(12.6000054068101,-1.89335265044601,0.64617044994032));
#10163=CARTESIAN_POINT('Ctrl Pts',(12.6000033360581,-1.88942004582711,0.653077891556402));
#10164=CARTESIAN_POINT('Ctrl Pts',(12.6000021947065,-1.88472046879005,0.659412676045522));
#10165=CARTESIAN_POINT('Ctrl Pts',(12.6000018847951,-1.88344439178375,0.661132761228218));
#10166=CARTESIAN_POINT('Ctrl Pts',(12.6000016718208,-1.88211149822114,0.662810505670431));
#10167=CARTESIAN_POINT('Ctrl Pts',(12.6000016744967,-1.88072259784382,0.664442334323417));
#10168=CARTESIAN_POINT('Ctrl Pts',(12.6000016781594,-1.87882150924004,0.666675936463772));
#10169=CARTESIAN_POINT('Ctrl Pts',(12.6000020841502,-1.87681550570489,0.668823545630641));
#10170=CARTESIAN_POINT('Ctrl Pts',(12.6000026366798,-1.87471194035196,0.670881441794774));
#10171=CARTESIAN_POINT('Ctrl Pts',(12.6000041308351,-1.86902346102148,0.676446422116204));
#10172=CARTESIAN_POINT('Ctrl Pts',(12.600006461375,-1.86269053299793,0.681293522350018));
#10173=CARTESIAN_POINT('Ctrl Pts',(12.6000072160154,-1.85587841208407,0.685370830723365));
#10174=CARTESIAN_POINT('Ctrl Pts',(12.6000077023835,-1.85148797774957,0.687998669380522));
#10175=CARTESIAN_POINT('Ctrl Pts',(12.6000076405209,-1.84689749427555,0.690306084934615));
#10176=CARTESIAN_POINT('Ctrl Pts',(12.6000070464578,-1.84214500723865,0.692269637845719));
#10177=CARTESIAN_POINT('Ctrl Pts',(12.6000061272438,-1.8347913233911,0.69530790964196));
#10178=CARTESIAN_POINT('Ctrl Pts',(12.6000039197963,-1.82713360831075,0.697490862850871));
#10179=CARTESIAN_POINT('Ctrl Pts',(12.6000021173902,-1.81932000848244,0.698749700991972));
#10180=CARTESIAN_POINT('Ctrl Pts',(12.6000009388424,-1.81421089282246,0.699572823470905));
#10181=CARTESIAN_POINT('Ctrl Pts',(12.6,-1.80903450780073,0.7));
#10182=CARTESIAN_POINT('Ctrl Pts',(12.6,-1.80383022254432,0.7));
#10183=CARTESIAN_POINT('Ctrl Pts',(12.4277899437912,-1.91498765980368,8.1061082099175E-6));
#10184=CARTESIAN_POINT('Ctrl Pts',(12.4185093097394,-1.90440735427916,0.201956437811591));
#10185=CARTESIAN_POINT('Ctrl Pts',(12.4092288296506,-1.89382707230216,0.403904777849331));
#10186=CARTESIAN_POINT('Ctrl Pts',(12.3999485057213,-1.88324681432718,0.605853126346544));
#10187=CARTESIAN_POINT('Ctrl Pts',(11.2514531524596,-1.79377193015415,-0.000335869645892519));
#10188=CARTESIAN_POINT('Ctrl Pts',(11.2440495594319,-1.78319067664719,0.201611894978303));
#10189=CARTESIAN_POINT('Ctrl Pts',(11.2366461029568,-1.77260943823668,0.403559665746509));
#10190=CARTESIAN_POINT('Ctrl Pts',(11.2292427771396,-1.76202821861547,0.605507441576721));
#10191=CARTESIAN_POINT('Ctrl Pts',(10.0755218259154,-1.69940246002113,-0.00057195363688788));
#10192=CARTESIAN_POINT('Ctrl Pts',(10.0699958446785,-1.68882059084335,0.201375418496625));
#10193=CARTESIAN_POINT('Ctrl Pts',(10.0644699805481,-1.67823873210945,0.403322794723726));
#10194=CARTESIAN_POINT('Ctrl Pts',(10.0589442279885,-1.66765688783508,0.605270174140068));
#10195=CARTESIAN_POINT('Ctrl Pts',(8.90001330805802,-1.62424530699552,-0.000736768987564917));
#10196=CARTESIAN_POINT('Ctrl Pts',(8.89636559238287,-1.61366301035882,0.201210329036737));
#10197=CARTESIAN_POINT('Ctrl Pts',(8.89271797406169,-1.60308072296431,0.403157429313698));
#10198=CARTESIAN_POINT('Ctrl Pts',(8.88907045450167,-1.59249844499155,0.605104531878289));
#10199=CARTESIAN_POINT('Ctrl Pts',(8.9000000009702,-1.5932011715731,0.605106081469384));
#10200=CARTESIAN_POINT('Ctrl Pts',(10.0684994345535,-1.66840362346204,0.605023135335662));
#10201=CARTESIAN_POINT('Ctrl Pts',(11.2356615742313,-1.76272273105624,0.604904457271936));
#10202=CARTESIAN_POINT('Ctrl Pts',(12.4,-1.8833055216247,0.604732563714112));
#10203=CARTESIAN_POINT('Ctrl Pts',(12.8889963716306,-1.96391015057091,2.25514051876985E-16));
#10204=CARTESIAN_POINT('Ctrl Pts',(12.8789974396847,-1.95334878321431,0.201594505485581));
#10205=CARTESIAN_POINT('Ctrl Pts',(12.8689986695879,-1.94278744208821,0.403189020401051));
#10206=CARTESIAN_POINT('Ctrl Pts',(12.8590000636394,-1.93222612769726,0.604783544887274));
#10207=CARTESIAN_POINT('Ctrl Pts',(12.792662965057,-1.95339909479377,-3.05216148415599E-5));
#10208=CARTESIAN_POINT('Ctrl Pts',(12.7828174539371,-1.94283764251598,0.201563933758495));
#10209=CARTESIAN_POINT('Ctrl Pts',(12.7729721028852,-1.93227621586528,0.403158398317997));
#10210=CARTESIAN_POINT('Ctrl Pts',(12.7631269141758,-1.92171481533493,0.604752872200892));
#10211=CARTESIAN_POINT('Ctrl Pts',(12.6963322449993,-1.94307475200589,-6.02899321993968E-5));
#10212=CARTESIAN_POINT('Ctrl Pts',(12.6866401583647,-1.93251321719056,0.201534116532542));
#10213=CARTESIAN_POINT('Ctrl Pts',(12.6769482300299,-1.92195170741534,0.403128531945268));
#10214=CARTESIAN_POINT('Ctrl Pts',(12.6672564622455,-1.91139022316239,0.604722956439736));
#10215=CARTESIAN_POINT('Ctrl Pts',(12.6000042264769,-1.9329329264796,-8.93242901516475E-5));
#10216=CARTESIAN_POINT('Ctrl Pts',(12.5904655680581,-1.92237131142302,0.201505034443145));
#10217=CARTESIAN_POINT('Ctrl Pts',(12.5809270661843,-1.91180972083551,0.403099401891705));
#10218=CARTESIAN_POINT('Ctrl Pts',(12.5713887230828,-1.90124815518829,0.604693778185974));
#10219=CARTESIAN_POINT('',(12.8572578715866,-1.93204080633595,0.60466226999893));
#10220=CARTESIAN_POINT('Ctrl Pts',(12.6000000000242,-1.90428042250026,0.604702508168697));
#10221=CARTESIAN_POINT('Ctrl Pts',(12.6857696261193,-1.91338852735451,0.604689390578107));
#10222=CARTESIAN_POINT('Ctrl Pts',(12.7715225733429,-1.92264108900731,0.604675979983877));
#10223=CARTESIAN_POINT('Ctrl Pts',(12.8572578715866,-1.93204080633595,0.60466226999893));
#10224=CARTESIAN_POINT('Ctrl Pts',(12.8572578715866,-1.93204080633595,0.604662269998931));
#10225=CARTESIAN_POINT('Ctrl Pts',(12.867837444884,-1.94266422047353,0.403108198925376));
#10226=CARTESIAN_POINT('Ctrl Pts',(12.8784169445746,-1.95328733374019,0.201554108835025));
#10227=CARTESIAN_POINT('Ctrl Pts',(12.8889963716306,-1.96391015057091,-1.13624387676481E-16));
#10228=CARTESIAN_POINT('Ctrl Pts',(12.4102890066107,-1.7839488953552,0.7));
#10229=CARTESIAN_POINT('Ctrl Pts',(11.2423261062923,-1.6629989551888,0.7));
#10230=CARTESIAN_POINT('Ctrl Pts',(10.0717272052363,-1.56846077660453,0.7));
#10231=CARTESIAN_POINT('Ctrl Pts',(8.89999999999993,-1.49312521822106,0.7));
#10232=CARTESIAN_POINT('Ctrl Pts',(12.4072999778185,-1.81281269415102,0.7));
#10233=CARTESIAN_POINT('Ctrl Pts',(11.2397765858669,-1.69187462084457,0.699998757165067));
#10234=CARTESIAN_POINT('Ctrl Pts',(10.0695527221263,-1.59734372851255,0.700000594792869));
#10235=CARTESIAN_POINT('Ctrl Pts',(8.89814271406455,-1.52201240649035,0.7));
#10236=CARTESIAN_POINT('Ctrl Pts',(12.4021203845267,-1.86282985658401,0.676448561733929));
#10237=CARTESIAN_POINT('Ctrl Pts',(11.2353531757414,-1.74191593276004,0.676505236381959));
#10238=CARTESIAN_POINT('Ctrl Pts',(10.0657879841113,-1.64739716848489,0.676543604639643));
#10239=CARTESIAN_POINT('Ctrl Pts',(8.89492397206972,-1.57207492202614,0.676570833338327));
#10240=CARTESIAN_POINT('Ctrl Pts',(12.400106093269,-1.88228102337346,0.626471792264191));
#10241=CARTESIAN_POINT('Ctrl Pts',(11.2336287644773,-1.76143987438699,0.626617923584012));
#10242=CARTESIAN_POINT('Ctrl Pts',(10.0643137348541,-1.66697079985262,0.626717999675944));
#10243=CARTESIAN_POINT('Ctrl Pts',(8.89366330605793,-1.59168261717615,0.626788336025017));
#10244=CARTESIAN_POINT('Ctrl Pts',(12.4,-1.8833055216247,0.604732563714112));
#10245=CARTESIAN_POINT('Ctrl Pts',(11.2335332423564,-1.7625023138725,0.604904771481731));
#10246=CARTESIAN_POINT('Ctrl Pts',(10.0642324382527,-1.66805889332185,0.605023569028795));
#10247=CARTESIAN_POINT('Ctrl Pts',(8.89359217382714,-1.59278896817116,0.605106535971077));
#10248=CARTESIAN_POINT('Ctrl Pts',(12.400000003046,-1.78288409409898,0.7));
#10249=CARTESIAN_POINT('Ctrl Pts',(11.235451325406,-1.66244391065713,0.7));
#10250=CARTESIAN_POINT('Ctrl Pts',(10.0682865064676,-1.56823955876321,0.7));
#10251=CARTESIAN_POINT('Ctrl Pts',(8.89999999999993,-1.49312521822106,0.7));
#10252=CARTESIAN_POINT('Ctrl Pts',(12.8681436286308,-1.83274446434879,0.7));
#10253=CARTESIAN_POINT('Ctrl Pts',(12.7787800350189,-1.82294762441299,0.7));
#10254=CARTESIAN_POINT('Ctrl Pts',(12.6893984576578,-1.8133105623702,0.7));
#10255=CARTESIAN_POINT('Ctrl Pts',(12.6,-1.80383022254431,0.7));
#10256=CARTESIAN_POINT('Ctrl Pts',(12.8649798835675,-1.86160311979107,0.7));
#10257=CARTESIAN_POINT('Ctrl Pts',(12.7756511334299,-1.85180730951691,0.699999896874207));
#10258=CARTESIAN_POINT('Ctrl Pts',(12.686303642571,-1.84217134991284,0.700000098415946));
#10259=CARTESIAN_POINT('Ctrl Pts',(12.5969393303221,-1.83269196733649,0.7));
#10260=CARTESIAN_POINT('Ctrl Pts',(12.8594976525144,-1.91161025179704,0.676425356750174));
#10261=CARTESIAN_POINT('Ctrl Pts',(12.7702288461641,-1.90181652272411,0.676430055978541));
#10262=CARTESIAN_POINT('Ctrl Pts',(12.6809412203008,-1.89218243450198,0.676434576658958));
#10263=CARTESIAN_POINT('Ctrl Pts',(12.5916356538948,-1.88270499442535,0.67643906321291));
#10264=CARTESIAN_POINT('Ctrl Pts',(12.8573684983393,-1.93103170500986,0.626412260100396));
#10265=CARTESIAN_POINT('Ctrl Pts',(12.7681225846323,-1.92124403769089,0.626424372515079));
#10266=CARTESIAN_POINT('Ctrl Pts',(12.6788572782757,-1.91161594713487,0.626436135819418));
#10267=CARTESIAN_POINT('Ctrl Pts',(12.5895741974899,-1.90214427893475,0.626447702441804));
#10268=CARTESIAN_POINT('Ctrl Pts',(12.8572578715866,-1.93204080633595,0.60466226999893));
#10269=CARTESIAN_POINT('Ctrl Pts',(12.7680127446979,-1.92225628370762,0.604676541242762));
#10270=CARTESIAN_POINT('Ctrl Pts',(12.6787484942245,-1.91263121188365,0.60469048808123));
#10271=CARTESIAN_POINT('Ctrl Pts',(12.5894662143615,-1.9031625467727,0.604704117718382));
#10272=CARTESIAN_POINT('',(12.8681436286308,-1.83274446434879,0.7));
#10273=CARTESIAN_POINT('Ctrl Pts',(12.8681436286308,-1.83274446434879,0.7));
#10274=CARTESIAN_POINT('Ctrl Pts',(12.7787800350189,-1.82294762441299,0.7));
#10275=CARTESIAN_POINT('Ctrl Pts',(12.6893984576578,-1.8133105623702,0.7));
#10276=CARTESIAN_POINT('Ctrl Pts',(12.6,-1.80383022254431,0.7));
#10277=CARTESIAN_POINT('Origin',(12.8681436286308,-1.83274446434879,0.6));
#10278=CARTESIAN_POINT('Origin',(6.87409734069396,-2.22251806091942E-16,
0.7));
#10279=CARTESIAN_POINT('Ctrl Pts',(8.9,1.49312521822106,0.7));
#10280=CARTESIAN_POINT('Ctrl Pts',(10.0682865064677,1.56823955876321,0.7));
#10281=CARTESIAN_POINT('Ctrl Pts',(11.2354513254061,1.66244391065714,0.7));
#10282=CARTESIAN_POINT('Ctrl Pts',(12.4000000030461,1.78288409409899,0.7));
#10283=CARTESIAN_POINT('Origin',(6.87409734069396,-2.22251806091942E-16,
0.7));
#10284=CARTESIAN_POINT('',(12.8681436286308,1.83274446434879,0.7));
#10285=CARTESIAN_POINT('Ctrl Pts',(12.6,1.80383022254432,0.7));
#10286=CARTESIAN_POINT('Ctrl Pts',(12.6893984576578,1.8133105623702,0.7));
#10287=CARTESIAN_POINT('Ctrl Pts',(12.7787800350189,1.82294762441299,0.7));
#10288=CARTESIAN_POINT('Ctrl Pts',(12.8681436286308,1.83274446434879,0.7));
#10289=CARTESIAN_POINT('',(12.8681436286308,1.1,0.7));
#10290=CARTESIAN_POINT('Ctrl Pts',(8.9,1.49312521822106,0.7));
#10291=CARTESIAN_POINT('Ctrl Pts',(10.0717272052363,1.56846077660453,0.7));
#10292=CARTESIAN_POINT('Ctrl Pts',(11.2423261062923,1.6629989551888,0.7));
#10293=CARTESIAN_POINT('Ctrl Pts',(12.4102890066107,1.7839488953552,0.7));
#10294=CARTESIAN_POINT('Ctrl Pts',(8.89814271406461,1.52201240649035,0.7));
#10295=CARTESIAN_POINT('Ctrl Pts',(10.0695527221263,1.59734372851256,0.700000594792869));
#10296=CARTESIAN_POINT('Ctrl Pts',(11.2397765858669,1.69187462084457,0.699998757165067));
#10297=CARTESIAN_POINT('Ctrl Pts',(12.4072999778185,1.81281269415102,0.7));
#10298=CARTESIAN_POINT('Ctrl Pts',(8.89492397206979,1.57207492202615,0.676570833338327));
#10299=CARTESIAN_POINT('Ctrl Pts',(10.0657879841114,1.64739716848489,0.676543604639644));
#10300=CARTESIAN_POINT('Ctrl Pts',(11.2353531757414,1.74191593276004,0.676505236381959));
#10301=CARTESIAN_POINT('Ctrl Pts',(12.4021203845267,1.86282985658401,0.676448561733929));
#10302=CARTESIAN_POINT('Ctrl Pts',(8.89366330605799,1.59168261717616,0.626788336025017));
#10303=CARTESIAN_POINT('Ctrl Pts',(10.0643137348542,1.66697079985262,0.626717999675944));
#10304=CARTESIAN_POINT('Ctrl Pts',(11.2336287644773,1.761439874387,0.626617923584012));
#10305=CARTESIAN_POINT('Ctrl Pts',(12.400106093269,1.88228102337346,0.626471792264191));
#10306=CARTESIAN_POINT('Ctrl Pts',(8.89359217382721,1.59278896817116,0.605106535971077));
#10307=CARTESIAN_POINT('Ctrl Pts',(10.0642324382527,1.66805889332185,0.605023569028795));
#10308=CARTESIAN_POINT('Ctrl Pts',(11.2335332423565,1.7625023138725,0.604904771481731));
#10309=CARTESIAN_POINT('Ctrl Pts',(12.4,1.8833055216247,0.604732563714112));
#10310=CARTESIAN_POINT('Ctrl Pts',(12.4,1.8833055216247,0.604732563714112));
#10311=CARTESIAN_POINT('Ctrl Pts',(11.2356615742313,1.76272273105624,0.604904457271936));
#10312=CARTESIAN_POINT('Ctrl Pts',(10.0684994345535,1.66840362346204,0.605023135335662));
#10313=CARTESIAN_POINT('Ctrl Pts',(8.90000000097019,1.5932011715731,0.605106081469384));
#10314=CARTESIAN_POINT('Ctrl Pts',(8.90001330805765,1.62424530699444,-0.000736768966955875));
#10315=CARTESIAN_POINT('Ctrl Pts',(8.89636559238262,1.6136630103581,0.201210329050476));
#10316=CARTESIAN_POINT('Ctrl Pts',(8.89271797406156,1.60308072296395,0.403157429320568));
#10317=CARTESIAN_POINT('Ctrl Pts',(8.88907045450167,1.59249844499155,0.605104531878289));
#10318=CARTESIAN_POINT('Ctrl Pts',(10.0755218259151,1.69940246002007,-0.000571953616278766));
#10319=CARTESIAN_POINT('Ctrl Pts',(10.0699958446785,1.68882059084265,0.201375418510364));
#10320=CARTESIAN_POINT('Ctrl Pts',(10.0644699805483,1.67823873210911,0.403322794730596));
#10321=CARTESIAN_POINT('Ctrl Pts',(10.0589442279888,1.6676568878351,0.605270174140069));
#10322=CARTESIAN_POINT('Ctrl Pts',(11.2514531524595,1.79377193015312,-0.000335869625283423));
#10323=CARTESIAN_POINT('Ctrl Pts',(11.244049559432,1.78319067664652,0.201611894992042));
#10324=CARTESIAN_POINT('Ctrl Pts',(11.2366461029572,1.77260943823637,0.403559665753379));
#10325=CARTESIAN_POINT('Ctrl Pts',(11.2292427771402,1.76202821861552,0.605507441576721));
#10326=CARTESIAN_POINT('Ctrl Pts',(12.4277899437912,1.9149876598027,8.10612881915578E-6));
#10327=CARTESIAN_POINT('Ctrl Pts',(12.4185093097397,1.90440735427854,0.201956437825331));
#10328=CARTESIAN_POINT('Ctrl Pts',(12.4092288296513,1.89382707230189,0.403904777856201));
#10329=CARTESIAN_POINT('Ctrl Pts',(12.3999485057223,1.88324681432728,0.605853126346545));
#10330=CARTESIAN_POINT('Ctrl Pts',(12.6000042264759,1.9329329264795,-8.93242901520291E-5));
#10331=CARTESIAN_POINT('Ctrl Pts',(12.5904655680574,1.92237131142328,0.201505034436202));
#10332=CARTESIAN_POINT('Ctrl Pts',(12.580927066184,1.91180972083614,0.403099401877819));
#10333=CARTESIAN_POINT('Ctrl Pts',(12.5713887230828,1.90124815518927,0.604693778165146));
#10334=CARTESIAN_POINT('Ctrl Pts',(12.6963322449987,1.94307475200582,-6.02899321996874E-5));
#10335=CARTESIAN_POINT('Ctrl Pts',(12.6866401583644,1.93251321719085,0.201534116525599));
#10336=CARTESIAN_POINT('Ctrl Pts',(12.6769482300299,1.921951707416,0.403128531931383));
#10337=CARTESIAN_POINT('Ctrl Pts',(12.6672564622458,1.91139022316341,0.604722956418908));
#10338=CARTESIAN_POINT('Ctrl Pts',(12.7926629650567,1.95339909479374,-3.05216148420481E-5));
#10339=CARTESIAN_POINT('Ctrl Pts',(12.7828174539371,1.94283764251631,0.201563933751552));
#10340=CARTESIAN_POINT('Ctrl Pts',(12.7729721028855,1.93227621586597,0.403158398304112));
#10341=CARTESIAN_POINT('Ctrl Pts',(12.7631269141765,1.92171481533599,0.604752872180064));
#10342=CARTESIAN_POINT('Ctrl Pts',(12.8889963716306,1.96391015057091,-1.66533453693773E-16));
#10343=CARTESIAN_POINT('Ctrl Pts',(12.878997439685,1.95334878321468,0.201594505478638));
#10344=CARTESIAN_POINT('Ctrl Pts',(12.8689986695886,1.94278744208894,0.403189020387166));
#10345=CARTESIAN_POINT('Ctrl Pts',(12.8590000636404,1.93222612769835,0.604783544866446));
#10346=CARTESIAN_POINT('',(12.8572578715866,1.93204080633595,0.60466226999893));
#10347=CARTESIAN_POINT('Ctrl Pts',(12.8889963716306,1.96391015057091,-3.88144377749811E-17));
#10348=CARTESIAN_POINT('Ctrl Pts',(12.8784169445746,1.95328733374019,0.201554108835021));
#10349=CARTESIAN_POINT('Ctrl Pts',(12.867837444884,1.94266422047353,0.403108198925375));
#10350=CARTESIAN_POINT('Ctrl Pts',(12.8572578715866,1.93204080633595,0.604662269998929));
#10351=CARTESIAN_POINT('Ctrl Pts',(12.8572578715866,1.93204080633595,0.60466226999893));
#10352=CARTESIAN_POINT('Ctrl Pts',(12.7715225733429,1.92264108900731,0.604675979983877));
#10353=CARTESIAN_POINT('Ctrl Pts',(12.6857696261193,1.91338852735451,0.604689390578107));
#10354=CARTESIAN_POINT('Ctrl Pts',(12.6000000000242,1.90428042250026,0.604702508168697));
#10355=CARTESIAN_POINT('Origin',(8.7,1.68851851851852,0.));
#10356=CARTESIAN_POINT('',(8.7,-1.5805153611151,0.605119933308333));
#10357=CARTESIAN_POINT('Ctrl Pts',(8.7,-1.5805153611151,0.605119933308333));
#10358=CARTESIAN_POINT('Ctrl Pts',(8.7,-1.58569938832865,0.504197823486131));
#10359=CARTESIAN_POINT('Ctrl Pts',(8.7,-1.59088373519313,0.403275164205241));
#10360=CARTESIAN_POINT('Ctrl Pts',(8.7,-1.60124586355191,0.201568897935389));
#10361=CARTESIAN_POINT('Ctrl Pts',(8.7,-1.60642370224807,0.10078416210737));
#10362=CARTESIAN_POINT('Ctrl Pts',(8.7,-1.61160179736194,0.));
#10363=CARTESIAN_POINT('',(8.7,-1.48045180431786,0.7));
#10364=CARTESIAN_POINT('Ctrl Pts',(8.70000000036779,-1.48045180452391,0.7));
#10365=CARTESIAN_POINT('Ctrl Pts',(8.70000000202598,-1.48836706478042,0.699999999180279));
#10366=CARTESIAN_POINT('Ctrl Pts',(8.70000127066624,-1.49622113223642,0.699007614827928));
#10367=CARTESIAN_POINT('Ctrl Pts',(8.70000237141531,-1.50387364922569,0.697121884028934));
#10368=CARTESIAN_POINT('Ctrl Pts',(8.70000291188189,-1.50763102664002,0.696195992283305));
#10369=CARTESIAN_POINT('Ctrl Pts',(8.70000341240591,-1.51133980954515,0.695053883793301));
#10370=CARTESIAN_POINT('Ctrl Pts',(8.70000377175886,-1.51498230649063,0.693702880475192));
#10371=CARTESIAN_POINT('Ctrl Pts',(8.70000450976793,-1.52246296255016,0.690928302676144));
#10372=CARTESIAN_POINT('Ctrl Pts',(8.70000452394134,-1.52958344744078,0.687306123577328));
#10373=CARTESIAN_POINT('Ctrl Pts',(8.70000379461986,-1.53619834892264,0.682919715776694));
#10374=CARTESIAN_POINT('Ctrl Pts',(8.70000333219987,-1.54039247012311,0.680138551763745));
#10375=CARTESIAN_POINT('Ctrl Pts',(8.70000258238552,-1.54438316197938,0.67704909562189));
#10376=CARTESIAN_POINT('Ctrl Pts',(8.70000192913237,-1.54812716280968,0.67366362845569));
#10377=CARTESIAN_POINT('Ctrl Pts',(8.70000138361353,-1.55125370412533,0.670836491537814));
#10378=CARTESIAN_POINT('Ctrl Pts',(8.70000090341281,-1.55418891097064,0.66782012731024));
#10379=CARTESIAN_POINT('Ctrl Pts',(8.7000009033621,-1.55691103280728,0.664625500020687));
#10380=CARTESIAN_POINT('Ctrl Pts',(8.7000009032669,-1.56202159382457,0.658627848677152));
#10381=CARTESIAN_POINT('Ctrl Pts',(8.70000241148087,-1.56638404855443,0.652003279246098));
#10382=CARTESIAN_POINT('Ctrl Pts',(8.70000292788623,-1.5699383402149,0.64491699469699));
#10383=CARTESIAN_POINT('Ctrl Pts',(8.70000298354275,-1.57032141040405,0.644153257609021));
#10384=CARTESIAN_POINT('Ctrl Pts',(8.70000303046442,-1.57069504840788,0.643384135640712));
#10385=CARTESIAN_POINT('Ctrl Pts',(8.70000306761332,-1.57105914547653,0.642609822781892));
#10386=CARTESIAN_POINT('Ctrl Pts',(8.70000341208914,-1.57443535963509,0.635429742901602));
#10387=CARTESIAN_POINT('Ctrl Pts',(8.70000263566904,-1.57695592401075,0.627888404173009));
#10388=CARTESIAN_POINT('Ctrl Pts',(8.70000151703179,-1.57856725066757,0.620153930269154));
#10389=CARTESIAN_POINT('Ctrl Pts',(8.70000080174396,-1.57959757782623,0.615208292159515));
#10390=CARTESIAN_POINT('Ctrl Pts',(8.7,-1.58025528705454,0.610183028431161));
#10391=CARTESIAN_POINT('Ctrl Pts',(8.7,-1.5805153611151,0.605119933308333));
#10392=CARTESIAN_POINT('',(8.7,1.48045180431904,0.7));
#10393=CARTESIAN_POINT('',(8.7,0.844259259259259,0.7));
#10394=CARTESIAN_POINT('',(8.7,1.5805153611151,0.605119933308333));
#10395=CARTESIAN_POINT('Ctrl Pts',(8.7,1.5805153611151,0.605119933308333));
#10396=CARTESIAN_POINT('Ctrl Pts',(8.7,1.58010890623597,0.61303275518587));
#10397=CARTESIAN_POINT('Ctrl Pts',(8.70000179355525,1.57873376841273,0.620855553142259));
#10398=CARTESIAN_POINT('Ctrl Pts',(8.7000025961206,1.5764741717406,0.62842799710221));
#10399=CARTESIAN_POINT('Ctrl Pts',(8.70000304562639,1.57520860278123,0.632669218617747));
#10400=CARTESIAN_POINT('Ctrl Pts',(8.70000324668712,1.57366457852079,0.636831947144834));
#10401=CARTESIAN_POINT('Ctrl Pts',(8.70000313318341,1.57185009366145,0.640886032861668));
#10402=CARTESIAN_POINT('Ctrl Pts',(8.70000293045856,1.56860930815545,0.648126888117959));
#10403=CARTESIAN_POINT('Ctrl Pts',(8.70000158438082,1.56454425420738,0.654942317779106));
#10404=CARTESIAN_POINT('Ctrl Pts',(8.70000106269264,1.55971945710293,0.661169479919421));
#10405=CARTESIAN_POINT('Ctrl Pts',(8.70000096439252,1.55881033523018,0.662342845179011));
#10406=CARTESIAN_POINT('Ctrl Pts',(8.70000090351839,1.55787410801649,0.663495254390581));
#10407=CARTESIAN_POINT('Ctrl Pts',(8.70000090409683,1.55691103285321,0.664625500020665));
#10408=CARTESIAN_POINT('Ctrl Pts',(8.70000090523835,1.55501044337284,0.666855993586132));
#10409=CARTESIAN_POINT('Ctrl Pts',(8.70000114361209,1.55300532702719,0.669000219206223));
#10410=CARTESIAN_POINT('Ctrl Pts',(8.70000146777886,1.55090303951829,0.671054438207787));
#10411=CARTESIAN_POINT('Ctrl Pts',(8.70000234447876,1.54521746205001,0.676610015749294));
#10412=CARTESIAN_POINT('Ctrl Pts',(8.70000370702799,1.53888821826629,0.681447385411957));
#10413=CARTESIAN_POINT('Ctrl Pts',(8.70000415375638,1.53207947242364,0.685512859850771));
#10414=CARTESIAN_POINT('Ctrl Pts',(8.70000443876751,1.52773551673798,0.688106618115728));
#10415=CARTESIAN_POINT('Ctrl Pts',(8.70000441165582,1.52319541573235,0.690385508075002));
#10416=CARTESIAN_POINT('Ctrl Pts',(8.70000407315693,1.51849599021366,0.692326230693156));
#10417=CARTESIAN_POINT('Ctrl Pts',(8.70000354533424,1.51116815716702,0.695352407250086));
#10418=CARTESIAN_POINT('Ctrl Pts',(8.70000225790696,1.50353761203248,0.697524030080351));
#10419=CARTESIAN_POINT('Ctrl Pts',(8.70000121423997,1.49575164755759,0.698771658000832));
#10420=CARTESIAN_POINT('Ctrl Pts',(8.70000053774506,1.49070486028667,0.699580358416591));
#10421=CARTESIAN_POINT('Ctrl Pts',(8.70000000144466,1.48559217323052,0.699999999467653));
#10422=CARTESIAN_POINT('Ctrl Pts',(8.70000000036779,1.48045180452391,0.7));
#10423=CARTESIAN_POINT('Ctrl Pts',(8.7,1.61160179736194,0.));
#10424=CARTESIAN_POINT('Ctrl Pts',(8.7,1.60642368739695,0.100784451162898));
#10425=CARTESIAN_POINT('Ctrl Pts',(8.7,1.60124583384883,0.201569476094892));
#10426=CARTESIAN_POINT('Ctrl Pts',(8.7,1.59088370548997,0.403275742430776));
#10427=CARTESIAN_POINT('Ctrl Pts',(8.7,1.58569937347746,0.504198112607714));
#10428=CARTESIAN_POINT('Ctrl Pts',(8.7,1.5805153611151,0.605119933308333));
#10429=CARTESIAN_POINT('Ctrl Pts',(8.7100201910492,-1.61222456240079,1.33887903992595E-6));
#10430=CARTESIAN_POINT('Ctrl Pts',(8.70667727354472,-1.60164608969543,0.201874135619687));
#10431=CARTESIAN_POINT('Ctrl Pts',(8.70333445073708,-1.59106762573893,0.40374693439627));
#10432=CARTESIAN_POINT('Ctrl Pts',(8.69999172399519,-1.58048917070122,0.605619735240497));
#10433=CARTESIAN_POINT('Ctrl Pts',(7.30266630830786,-1.52469223633113,-0.000186944012493601));
#10434=CARTESIAN_POINT('Ctrl Pts',(7.3015714609838,-1.51411327886182,0.201685539385837));
#10435=CARTESIAN_POINT('Ctrl Pts',(7.30047669312962,-1.50353432123569,0.403558023359813));
#10436=CARTESIAN_POINT('Ctrl Pts',(7.2993819983171,-1.49295537435081,0.605430507723141));
#10437=CARTESIAN_POINT('Ctrl Pts',(5.89591889571946,-1.46411055243784,-0.000276130330627546));
#10438=CARTESIAN_POINT('Ctrl Pts',(5.8970730573458,-1.45353136553189,0.201596203763285));
#10439=CARTESIAN_POINT('Ctrl Pts',(5.89822728315403,-1.44295217665945,0.403468537584815));
#10440=CARTESIAN_POINT('Ctrl Pts',(5.89938156763751,-1.43237299696387,0.60534087113472));
#10441=CARTESIAN_POINT('Ctrl Pts',(4.48978738186403,-1.41740792524342,-0.000330195618103912));
#10442=CARTESIAN_POINT('Ctrl Pts',(4.49319153668887,-1.4068286019831,0.201542048187911));
#10443=CARTESIAN_POINT('Ctrl Pts',(4.49659574248722,-1.39624928130228,0.403414291272231));
#10444=CARTESIAN_POINT('Ctrl Pts',(4.5,-1.3856699632509,0.605286533625018));
#10445=CARTESIAN_POINT('Ctrl Pts',(4.50000000014037,-1.38566996330298,0.605286533623957));
#10446=CARTESIAN_POINT('Ctrl Pts',(5.90109530155974,-1.43243455365708,0.605259331490037));
#10447=CARTESIAN_POINT('Ctrl Pts',(7.30150776148394,-1.49309969195427,0.605214402664297));
#10448=CARTESIAN_POINT('Ctrl Pts',(8.7,-1.5805153611151,0.605119933308333));
#10449=CARTESIAN_POINT('Ctrl Pts',(8.7062300060629,-1.48084102486261,0.7));
#10450=CARTESIAN_POINT('Ctrl Pts',(7.30535837857749,-1.39328148786737,0.7));
#10451=CARTESIAN_POINT('Ctrl Pts',(5.90286553803659,-1.3325543763676,0.7));
#10452=CARTESIAN_POINT('Ctrl Pts',(4.5,-1.28575421950843,0.7));
#10453=CARTESIAN_POINT('Ctrl Pts',(8.7044244076592,-1.50972892972339,0.7));
#10454=CARTESIAN_POINT('Ctrl Pts',(7.30392377861185,-1.42217417124324,0.699999322371676));
#10455=CARTESIAN_POINT('Ctrl Pts',(5.90170976758769,-1.36144968116949,0.700000194339816));
#10456=CARTESIAN_POINT('Ctrl Pts',(4.49903600403804,-1.314650633636,0.7));
#10457=CARTESIAN_POINT('Ctrl Pts',(8.70129509098077,-1.55979510296572,0.676577193851887));
#10458=CARTESIAN_POINT('Ctrl Pts',(7.30143307762773,-1.47225060169427,0.676608218952397));
#10459=CARTESIAN_POINT('Ctrl Pts',(5.89970879741633,-1.41153023905743,0.676622651488038));
#10460=CARTESIAN_POINT('Ctrl Pts',(4.49736521340071,-1.36473368385825,0.676631564755462));
#10461=CARTESIAN_POINT('Ctrl Pts',(8.70006933407556,-1.57940608001781,0.626799670546273));
#10462=CARTESIAN_POINT('Ctrl Pts',(7.3004573192207,-1.49190036240803,0.626879818917698));
#10463=CARTESIAN_POINT('Ctrl Pts',(5.89892183391985,-1.43119871194172,0.62691759730524));
#10464=CARTESIAN_POINT('Ctrl Pts',(4.49670869913724,-1.38441313147668,0.626940642142451));
#10465=CARTESIAN_POINT('Ctrl Pts',(8.7,-1.5805153611151,0.605119933308333));
#10466=CARTESIAN_POINT('Ctrl Pts',(7.30039998287682,-1.49303044794594,0.605214477495697));
#10467=CARTESIAN_POINT('Ctrl Pts',(5.89887670103551,-1.4323384618751,0.605259402637312));
#10468=CARTESIAN_POINT('Ctrl Pts',(4.49667047719213,-1.38555885946567,0.605286598232956));
#10469=CARTESIAN_POINT('Ctrl Pts',(8.70000000036771,-1.48045180452391,0.7));
#10470=CARTESIAN_POINT('Ctrl Pts',(7.30120024114866,-1.39310147361351,0.7));
#10471=CARTESIAN_POINT('Ctrl Pts',(5.90078591724148,-1.332484999384,0.7));
#10472=CARTESIAN_POINT('Ctrl Pts',(4.5,-1.28575421950843,0.7));
#10473=CARTESIAN_POINT('Origin',(6.87409734069396,-2.22251806091942E-16,
0.7));
#10474=CARTESIAN_POINT('Ctrl Pts',(4.5,1.28575421950843,0.7));
#10475=CARTESIAN_POINT('Ctrl Pts',(5.9007859172415,1.332484999384,0.7));
#10476=CARTESIAN_POINT('Ctrl Pts',(7.30120024114871,1.39310147361351,0.7));
#10477=CARTESIAN_POINT('Ctrl Pts',(8.70000000036779,1.48045180452391,0.7));
#10478=CARTESIAN_POINT('Ctrl Pts',(4.5,1.28575421950843,0.7));
#10479=CARTESIAN_POINT('Ctrl Pts',(5.90286553803659,1.3325543763676,0.7));
#10480=CARTESIAN_POINT('Ctrl Pts',(7.30535837857749,1.39328148786737,0.7));
#10481=CARTESIAN_POINT('Ctrl Pts',(8.7062300060629,1.48084102486261,0.7));
#10482=CARTESIAN_POINT('Ctrl Pts',(4.49903600403804,1.314650633636,0.7));
#10483=CARTESIAN_POINT('Ctrl Pts',(5.90170976758769,1.36144968116949,0.700000194339816));
#10484=CARTESIAN_POINT('Ctrl Pts',(7.30392377861185,1.42217417124324,0.699999322371676));
#10485=CARTESIAN_POINT('Ctrl Pts',(8.7044244076592,1.50972892972339,0.7));
#10486=CARTESIAN_POINT('Ctrl Pts',(4.49736521340071,1.36473368385825,0.676631564755462));
#10487=CARTESIAN_POINT('Ctrl Pts',(5.89970879741633,1.41153023905743,0.676622651488038));
#10488=CARTESIAN_POINT('Ctrl Pts',(7.30143307762774,1.47225060169427,0.676608218952397));
#10489=CARTESIAN_POINT('Ctrl Pts',(8.70129509098078,1.55979510296572,0.676577193851887));
#10490=CARTESIAN_POINT('Ctrl Pts',(4.49670869913724,1.38441313147668,0.626940642142451));
#10491=CARTESIAN_POINT('Ctrl Pts',(5.89892183391985,1.43119871194172,0.626917597305239));
#10492=CARTESIAN_POINT('Ctrl Pts',(7.3004573192207,1.49190036240803,0.626879818917698));
#10493=CARTESIAN_POINT('Ctrl Pts',(8.70006933407556,1.57940608001781,0.626799670546273));
#10494=CARTESIAN_POINT('Ctrl Pts',(4.49667047719213,1.38555885946567,0.605286598232956));
#10495=CARTESIAN_POINT('Ctrl Pts',(5.89887670103551,1.4323384618751,0.605259402637312));
#10496=CARTESIAN_POINT('Ctrl Pts',(7.30039998287682,1.49303044794594,0.605214477495697));
#10497=CARTESIAN_POINT('Ctrl Pts',(8.7,1.5805153611151,0.605119933308333));
#10498=CARTESIAN_POINT('Ctrl Pts',(8.7,1.5805153611151,0.605119933308333));
#10499=CARTESIAN_POINT('Ctrl Pts',(7.30150776148394,1.49309969195427,0.605214402664297));
#10500=CARTESIAN_POINT('Ctrl Pts',(5.90109530155974,1.43243455365708,0.605259331490037));
#10501=CARTESIAN_POINT('Ctrl Pts',(4.50000000014037,1.38566996330298,0.605286533623957));
#10502=CARTESIAN_POINT('Ctrl Pts',(4.48978738186405,1.41740792524342,-0.00033019561810394));
#10503=CARTESIAN_POINT('Ctrl Pts',(4.49319153668889,1.40682860198312,0.201542048187577));
#10504=CARTESIAN_POINT('Ctrl Pts',(4.49659574248723,1.39624928130232,0.403414291271564));
#10505=CARTESIAN_POINT('Ctrl Pts',(4.5,1.38566996325095,0.605286533624017));
#10506=CARTESIAN_POINT('Ctrl Pts',(5.89591889571947,1.46411055243784,-0.000276130330627574));
#10507=CARTESIAN_POINT('Ctrl Pts',(5.89707305734581,1.45353136553191,0.201596203762952));
#10508=CARTESIAN_POINT('Ctrl Pts',(5.89822728315404,1.44295217665948,0.403468537584147));
#10509=CARTESIAN_POINT('Ctrl Pts',(5.89938156763751,1.43237299696393,0.605340871133719));
#10510=CARTESIAN_POINT('Ctrl Pts',(7.30266630830786,1.52469223633113,-0.000186944012493549));
#10511=CARTESIAN_POINT('Ctrl Pts',(7.3015714609838,1.51411327886184,0.201685539385503));
#10512=CARTESIAN_POINT('Ctrl Pts',(7.30047669312963,1.50353432123572,0.403558023359145));
#10513=CARTESIAN_POINT('Ctrl Pts',(7.29938199831711,1.49295537435086,0.60543050772214));
#10514=CARTESIAN_POINT('Ctrl Pts',(8.7100201910492,1.61222456240079,1.33887903989646E-6));
#10515=CARTESIAN_POINT('Ctrl Pts',(8.70667727354472,1.60164608969545,0.201874135619353));
#10516=CARTESIAN_POINT('Ctrl Pts',(8.7033344507371,1.59106762573896,0.403746934395602));
#10517=CARTESIAN_POINT('Ctrl Pts',(8.6999917239952,1.58048917070127,0.605619735239495));
#10518=CARTESIAN_POINT('Origin',(4.3,1.48481481481482,0.));
#10519=CARTESIAN_POINT('',(4.3,-1.37908752581626,0.605290299758539));
#10520=CARTESIAN_POINT('Ctrl Pts',(4.3,-1.37908752581626,0.605290299758539));
#10521=CARTESIAN_POINT('Ctrl Pts',(4.3,-1.38444464017247,0.504222347694443));
#10522=CARTESIAN_POINT('Ctrl Pts',(4.3,-1.38980163214303,0.403154389143214));
#10523=CARTESIAN_POINT('Ctrl Pts',(4.3,-1.40049562949383,0.201390955816302));
#10524=CARTESIAN_POINT('Ctrl Pts',(4.3,-1.40583263576898,0.100695481088992));
#10525=CARTESIAN_POINT('Ctrl Pts',(4.3,-1.41116952203211,0.));
#10526=CARTESIAN_POINT('Ctrl Pts',(4.30000000005992,-1.27917501058303,0.7));
#10527=CARTESIAN_POINT('Ctrl Pts',(4.30000000048661,-1.28708628524264,0.699999999884766));
#10528=CARTESIAN_POINT('Ctrl Pts',(4.30000064978116,-1.29493415608545,0.69900616264686));
#10529=CARTESIAN_POINT('Ctrl Pts',(4.30000121018478,-1.30257825621016,0.697119208693397));
#10530=CARTESIAN_POINT('Ctrl Pts',(4.30000152558655,-1.30688044586137,0.696057208766858));
#10531=CARTESIAN_POINT('Ctrl Pts',(4.30000181105247,-1.31111814675806,0.694711271736901));
#10532=CARTESIAN_POINT('Ctrl Pts',(4.30000199036827,-1.31526464671957,0.693092387263961));
#10533=CARTESIAN_POINT('Ctrl Pts',(4.30000231141323,-1.32268849323592,0.690193954859197));
#10534=CARTESIAN_POINT('Ctrl Pts',(4.30000222777046,-1.32973966400828,0.686455190804221));
#10535=CARTESIAN_POINT('Ctrl Pts',(4.30000179417102,-1.33627196700415,0.681957645816867));
#10536=CARTESIAN_POINT('Ctrl Pts',(4.30000155535849,-1.33986974800182,0.679480543652151));
#10537=CARTESIAN_POINT('Ctrl Pts',(4.30000121902461,-1.34330986828215,0.67677238407294));
#10538=CARTESIAN_POINT('Ctrl Pts',(4.30000092191081,-1.34656397897095,0.673841242448196));
#10539=CARTESIAN_POINT('Ctrl Pts',(4.30000063243573,-1.34973442737118,0.670985459666446));
#10540=CARTESIAN_POINT('Ctrl Pts',(4.30000037658882,-1.35270906921767,0.667935271966333));
#10541=CARTESIAN_POINT('Ctrl Pts',(4.30000037869864,-1.35546536049262,0.66470214425512));
#10542=CARTESIAN_POINT('Ctrl Pts',(4.30000038260995,-1.36057515211559,0.658708362304413));
#10543=CARTESIAN_POINT('Ctrl Pts',(4.30000117797282,-1.36493744806469,0.652087250959406));
#10544=CARTESIAN_POINT('Ctrl Pts',(4.30000145944905,-1.36849285270534,0.645004510397983));
#10545=CARTESIAN_POINT('Ctrl Pts',(4.30000148826005,-1.36885677248754,0.644279543857467));
#10546=CARTESIAN_POINT('Ctrl Pts',(4.30000151299237,-1.36921219826683,0.643549721050429));
#10547=CARTESIAN_POINT('Ctrl Pts',(4.30000153317099,-1.36955903781249,0.642815208524159));
#10548=CARTESIAN_POINT('Ctrl Pts',(4.30000173031152,-1.37294758118467,0.635639188419686));
#10549=CARTESIAN_POINT('Ctrl Pts',(4.30000134819424,-1.37548140076902,0.628100134775109));
#10550=CARTESIAN_POINT('Ctrl Pts',(4.30000077902196,-1.37710733725971,0.620366659714886));
#10551=CARTESIAN_POINT('Ctrl Pts',(4.30000041405338,-1.37814993145247,0.615407747584041));
#10552=CARTESIAN_POINT('Ctrl Pts',(4.3,-1.37881837002099,0.610368224776708));
#10553=CARTESIAN_POINT('Ctrl Pts',(4.3,-1.37908752581626,0.605290299758539));
#10554=CARTESIAN_POINT('',(4.3,1.37908752581626,0.605290299758539));
#10555=CARTESIAN_POINT('Ctrl Pts',(4.3,1.37908752581626,0.605290299758539));
#10556=CARTESIAN_POINT('Ctrl Pts',(4.3,1.37866806817032,0.613203837240499));
#10557=CARTESIAN_POINT('Ctrl Pts',(4.30000092021544,1.37728139671899,0.621026590428679));
#10558=CARTESIAN_POINT('Ctrl Pts',(4.30000132151137,1.37501133257008,0.628597948954885));
#10559=CARTESIAN_POINT('Ctrl Pts',(4.30000154544343,1.37374458621782,0.632822935636113));
#10560=CARTESIAN_POINT('Ctrl Pts',(4.30000164013187,1.37220176226583,0.636969676056352));
#10561=CARTESIAN_POINT('Ctrl Pts',(4.30000157305315,1.37039070587839,0.641008268098125));
#10562=CARTESIAN_POINT('Ctrl Pts',(4.30000145288191,1.36714620633991,0.648243387946652));
#10563=CARTESIAN_POINT('Ctrl Pts',(4.30000073948134,1.36307905360626,0.655053358422861));
#10564=CARTESIAN_POINT('Ctrl Pts',(4.3000004635866,1.35825284513469,0.661274801567968));
#10565=CARTESIAN_POINT('Ctrl Pts',(4.30000041199046,1.35735027731582,0.662438297592388));
#10566=CARTESIAN_POINT('Ctrl Pts',(4.30000037986005,1.35642103364291,0.663581140343808));
#10567=CARTESIAN_POINT('Ctrl Pts',(4.30000037943224,1.35546536051643,0.664702144255114));
#10568=CARTESIAN_POINT('Ctrl Pts',(4.300000378582,1.3535659898678,0.666930104702213));
#10569=CARTESIAN_POINT('Ctrl Pts',(4.3000005018795,1.35156225525783,0.669071850305581));
#10570=CARTESIAN_POINT('Ctrl Pts',(4.30000067038034,1.34946148384904,0.671123623013939));
#10571=CARTESIAN_POINT('Ctrl Pts',(4.30000112630012,1.34377733881547,0.676675190215126));
#10572=CARTESIAN_POINT('Ctrl Pts',(4.30000183907902,1.33744971106208,0.68150833207295));
#10573=CARTESIAN_POINT('Ctrl Pts',(4.30000208123143,1.33064243458576,0.685568782013219));
#10574=CARTESIAN_POINT('Ctrl Pts',(4.30000223513396,1.3263159977886,0.688149444058562));
#10575=CARTESIAN_POINT('Ctrl Pts',(4.3000022300233,1.32179485563522,0.690417305529342));
#10576=CARTESIAN_POINT('Ctrl Pts',(4.30000206344016,1.31711540146937,0.692349146556373));
#10577=CARTESIAN_POINT('Ctrl Pts',(4.3000018029167,1.30979708846622,0.695370400063095));
#10578=CARTESIAN_POINT('Ctrl Pts',(4.30000114702936,1.30217656646843,0.69753735975804));
#10579=CARTESIAN_POINT('Ctrl Pts',(4.3000006156201,1.29440092269557,0.69878042986007));
#10580=CARTESIAN_POINT('Ctrl Pts',(4.30000027236218,1.28937833178082,0.699583377215073));
#10581=CARTESIAN_POINT('Ctrl Pts',(4.30000000033581,1.28429042584107,0.69999999992549));
#10582=CARTESIAN_POINT('Ctrl Pts',(4.30000000005992,1.27917501058303,0.7));
#10583=CARTESIAN_POINT('Ctrl Pts',(4.3,1.41116952203211,0.));
#10584=CARTESIAN_POINT('Ctrl Pts',(4.3,1.40583262613343,0.100695662891028));
#10585=CARTESIAN_POINT('Ctrl Pts',(4.3,1.40049561022223,0.201391319421434));
#10586=CARTESIAN_POINT('Ctrl Pts',(4.3,1.38980161287056,0.403154752748307));
#10587=CARTESIAN_POINT('Ctrl Pts',(4.3,1.38444463053604,0.504222529496425));
#10588=CARTESIAN_POINT('Ctrl Pts',(4.3,1.37908752581626,0.605290299758539));
#10589=CARTESIAN_POINT('Ctrl Pts',(4.3,-1.41116952203217,-1.08233907947231E-12));
#10590=CARTESIAN_POINT('Ctrl Pts',(4.30370667985561,-1.40059355144761,0.201807922462111));
#10591=CARTESIAN_POINT('Ctrl Pts',(4.30741340932898,-1.39001758331341,0.403615844144917));
#10592=CARTESIAN_POINT('Ctrl Pts',(4.31112018914117,-1.37944161767694,0.605423765036612));
#10593=CARTESIAN_POINT('Ctrl Pts',(3.22410085073145,-1.37636920007795,-3.90459529712038E-5));
#10594=CARTESIAN_POINT('Ctrl Pts',(3.2295286994181,-1.36579313421488,0.201768811380596));
#10595=CARTESIAN_POINT('Ctrl Pts',(3.23495659078338,-1.35521706809947,0.403576667516588));
#10596=CARTESIAN_POINT('Ctrl Pts',(3.24038452463065,-1.34464100578453,0.605384522622892));
#10597=CARTESIAN_POINT('Ctrl Pts',(2.14856196511704,-1.34935185539723,-5.92140864038068E-5));
#10598=CARTESIAN_POINT('Ctrl Pts',(2.15571155670467,-1.33877574824886,0.201748609775608));
#10599=CARTESIAN_POINT('Ctrl Pts',(2.16286118630165,-1.32819964054015,0.403556432267456));
#10600=CARTESIAN_POINT('Ctrl Pts',(2.17001085376486,-1.31762353633116,0.605364253566666));
#10601=CARTESIAN_POINT('Ctrl Pts',(1.073384157387,-1.32427529283232,-8.86713468529234E-5));
#10602=CARTESIAN_POINT('Ctrl Pts',(1.08225606990756,-1.31369916974321,0.201719104822629));
#10603=CARTESIAN_POINT('Ctrl Pts',(1.09112801825726,-1.30312304798914,0.403526879488275));
#10604=CARTESIAN_POINT('Ctrl Pts',(1.10000000295732,-1.29254692759565,0.605334652628532));
#10605=CARTESIAN_POINT('Ctrl Pts',(1.10000000298281,-1.29254692760111,0.605334652628557));
#10606=CARTESIAN_POINT('Ctrl Pts',(2.16694388170712,-1.31755402957363,0.605319894542965));
#10607=CARTESIAN_POINT('Ctrl Pts',(3.23367147240841,-1.34448060345116,0.605309774863278));
#10608=CARTESIAN_POINT('Ctrl Pts',(4.3,-1.37908752581626,0.605290299758539));
#10609=CARTESIAN_POINT('Ctrl Pts',(4.30323908112369,-1.2792801058419,0.7));
#10610=CARTESIAN_POINT('Ctrl Pts',(3.23565147654712,-1.24463335454069,0.7));
#10611=CARTESIAN_POINT('Ctrl Pts',(2.1678436779024,-1.21768649131741,0.7));
#10612=CARTESIAN_POINT('Ctrl Pts',(1.09999999999999,-1.19266190204553,0.7));
#10613=CARTESIAN_POINT('Ctrl Pts',(4.30230129178181,-1.30817667592415,0.7));
#10614=CARTESIAN_POINT('Ctrl Pts',(3.23485320804887,-1.27353066282864,0.699999860738333));
#10615=CARTESIAN_POINT('Ctrl Pts',(2.16713169816659,-1.24658393122273,0.700000105496227));
#10616=CARTESIAN_POINT('Ctrl Pts',(1.0993228455422,-1.22155728565617,0.7));
#10617=CARTESIAN_POINT('Ctrl Pts',(4.30067574076257,-1.35826558912881,0.676637683834297));
#10618=CARTESIAN_POINT('Ctrl Pts',(3.23346787205668,-1.32362126434549,0.676644071225102));
#10619=CARTESIAN_POINT('Ctrl Pts',(2.16589795861771,-1.29667457247055,0.676647306834711));
#10620=CARTESIAN_POINT('Ctrl Pts',(1.09814906228501,-1.27164470234869,0.676652147774997));
#10621=CARTESIAN_POINT('Ctrl Pts',(4.30003720890047,-1.37794098943329,0.626943772371838));
#10622=CARTESIAN_POINT('Ctrl Pts',(3.23292426239396,-1.34330449078822,0.626960286972675));
#10623=CARTESIAN_POINT('Ctrl Pts',(2.16541285690349,-1.31636171257899,0.6269687859393));
#10624=CARTESIAN_POINT('Ctrl Pts',(1.09768760301306,-1.29133598921902,0.626981304916489));
#10625=CARTESIAN_POINT('Ctrl Pts',(4.3,-1.37908752581626,0.605290299758539));
#10626=CARTESIAN_POINT('Ctrl Pts',(3.23289209128077,-1.34445530919946,0.605309789097661));
#10627=CARTESIAN_POINT('Ctrl Pts',(2.16538453588699,-1.31751467232976,0.605319909330946));
#10628=CARTESIAN_POINT('Ctrl Pts',(1.09766050997011,-1.29249209748956,0.605334684996117));
#10629=CARTESIAN_POINT('Ctrl Pts',(1.09999999999999,1.19266190204553,0.7));
#10630=CARTESIAN_POINT('Ctrl Pts',(2.1678436779024,1.21768649131741,0.7));
#10631=CARTESIAN_POINT('Ctrl Pts',(3.23565147654712,1.24463335454069,0.7));
#10632=CARTESIAN_POINT('Ctrl Pts',(4.30323908112369,1.2792801058419,0.7));
#10633=CARTESIAN_POINT('Ctrl Pts',(1.0993228455422,1.22155728565617,0.7));
#10634=CARTESIAN_POINT('Ctrl Pts',(2.16713169816659,1.24658393122273,0.700000105496227));
#10635=CARTESIAN_POINT('Ctrl Pts',(3.23485320804887,1.27353066282864,0.699999860738333));
#10636=CARTESIAN_POINT('Ctrl Pts',(4.30230129178181,1.30817667592415,0.7));
#10637=CARTESIAN_POINT('Ctrl Pts',(1.09814906228501,1.27164470234869,0.676652147774997));
#10638=CARTESIAN_POINT('Ctrl Pts',(2.16589795861771,1.29667457247055,0.676647306834711));
#10639=CARTESIAN_POINT('Ctrl Pts',(3.23346787205668,1.32362126434549,0.676644071225102));
#10640=CARTESIAN_POINT('Ctrl Pts',(4.30067574076257,1.35826558912881,0.676637683834297));
#10641=CARTESIAN_POINT('Ctrl Pts',(1.09768760301306,1.29133598921902,0.626981304916489));
#10642=CARTESIAN_POINT('Ctrl Pts',(2.16541285690349,1.31636171257899,0.6269687859393));
#10643=CARTESIAN_POINT('Ctrl Pts',(3.23292426239396,1.34330449078822,0.626960286972675));
#10644=CARTESIAN_POINT('Ctrl Pts',(4.30003720890047,1.37794098943329,0.626943772371838));
#10645=CARTESIAN_POINT('Ctrl Pts',(1.09766050997011,1.29249209748956,0.605334684996117));
#10646=CARTESIAN_POINT('Ctrl Pts',(2.16538453588699,1.31751467232976,0.605319909330946));
#10647=CARTESIAN_POINT('Ctrl Pts',(3.23289209128077,1.34445530919946,0.605309789097661));
#10648=CARTESIAN_POINT('Ctrl Pts',(4.3,1.37908752581626,0.605290299758539));
#10649=CARTESIAN_POINT('Ctrl Pts',(4.3,1.37908752581626,0.605290299758539));
#10650=CARTESIAN_POINT('Ctrl Pts',(3.23367147240841,1.34448060345116,0.605309774863278));
#10651=CARTESIAN_POINT('Ctrl Pts',(2.16694388170711,1.31755402957363,0.605319894542965));
#10652=CARTESIAN_POINT('Ctrl Pts',(1.10000000298281,1.29254692760111,0.605334652628557));
#10653=CARTESIAN_POINT('Ctrl Pts',(1.07338415738705,1.32427529283227,-8.86713457716078E-5));
#10654=CARTESIAN_POINT('Ctrl Pts',(1.08225606990759,1.31369916974318,0.201719104823349));
#10655=CARTESIAN_POINT('Ctrl Pts',(1.09112801825728,1.30312304798912,0.403526879488635));
#10656=CARTESIAN_POINT('Ctrl Pts',(1.10000000295732,1.29254692759565,0.605334652628532));
#10657=CARTESIAN_POINT('Ctrl Pts',(2.14856196511707,1.34935185539717,-5.92140853224782E-5));
#10658=CARTESIAN_POINT('Ctrl Pts',(2.15571155670469,1.33877574824882,0.201748609776328));
#10659=CARTESIAN_POINT('Ctrl Pts',(2.16286118630166,1.32819964054013,0.403556432267816));
#10660=CARTESIAN_POINT('Ctrl Pts',(2.17001085376486,1.31762353633116,0.605364253566666));
#10661=CARTESIAN_POINT('Ctrl Pts',(3.22410085073147,1.37636920007789,-3.90459518899617E-5));
#10662=CARTESIAN_POINT('Ctrl Pts',(3.22952869941811,1.36579313421484,0.201768811381317));
#10663=CARTESIAN_POINT('Ctrl Pts',(3.23495659078338,1.35521706809945,0.403576667516948));
#10664=CARTESIAN_POINT('Ctrl Pts',(3.24038452463064,1.34464100578453,0.605384522622892));
#10665=CARTESIAN_POINT('Ctrl Pts',(4.3,1.41116952203211,-1.07899800205757E-15));
#10666=CARTESIAN_POINT('Ctrl Pts',(4.3037066798556,1.40059355144758,0.201807922462832));
#10667=CARTESIAN_POINT('Ctrl Pts',(4.30741340932897,1.39001758331339,0.403615844145277));
#10668=CARTESIAN_POINT('Ctrl Pts',(4.31112018914115,1.37944161767694,0.605423765036611));
#10669=CARTESIAN_POINT('Origin',(0.9,1.39290118819044,0.));
#10670=CARTESIAN_POINT('',(0.900000001878204,-1.28788040994396,0.605337476551879));
#10671=CARTESIAN_POINT('Ctrl Pts',(0.900000001878204,-1.28788040994396,
0.605337476551879));
#10672=CARTESIAN_POINT('Ctrl Pts',(0.900000001878204,-1.29328625806092,
0.504228160928694));
#10673=CARTESIAN_POINT('Ctrl Pts',(0.899999999999999,-1.29869191435855,
0.403118132397745));
#10674=CARTESIAN_POINT('Ctrl Pts',(0.899999999999999,-1.30947917558554,
0.201339438823693));
#10675=CARTESIAN_POINT('Ctrl Pts',(0.9,-1.31486085669789,0.100669384150719));
#10676=CARTESIAN_POINT('Ctrl Pts',(0.9,-1.32024227787037,0.));
#10677=CARTESIAN_POINT('',(0.9,-1.18799600975353,0.7));
#10678=CARTESIAN_POINT('Ctrl Pts',(0.900000000000324,-1.18799600975363,
0.7));
#10679=CARTESIAN_POINT('Ctrl Pts',(0.900000000063601,-1.19590581948314,
0.699999999935493));
#10680=CARTESIAN_POINT('Ctrl Pts',(0.900000451671414,-1.20375274583281,
0.699006541951706));
#10681=CARTESIAN_POINT('Ctrl Pts',(0.900000834722547,-1.21139610511184,
0.697120084132161));
#10682=CARTESIAN_POINT('Ctrl Pts',(0.900001049758257,-1.21568690349652,
0.696061072005504));
#10683=CARTESIAN_POINT('Ctrl Pts',(0.900001241882928,-1.21991360580594,
0.694719604949841));
#10684=CARTESIAN_POINT('Ctrl Pts',(0.900001357948449,-1.22404965357203,
0.693106547509926));
#10685=CARTESIAN_POINT('Ctrl Pts',(0.900001566283472,-1.23147376710855,
0.690211145364658));
#10686=CARTESIAN_POINT('Ctrl Pts',(0.900001483882417,-1.23852542365708,
0.686475281350474));
#10687=CARTESIAN_POINT('Ctrl Pts',(0.90000115772027,-1.24505817055452,0.681980323292531));
#10688=CARTESIAN_POINT('Ctrl Pts',(0.90000097852015,-1.2486473946309,0.67951070187031));
#10689=CARTESIAN_POINT('Ctrl Pts',(0.900000731874511,-1.25207971535834,
0.676811055842604));
#10690=CARTESIAN_POINT('Ctrl Pts',(0.90000051586667,-1.25532695882913,0.673889369778116));
#10691=CARTESIAN_POINT('Ctrl Pts',(0.900000304282776,-1.25850769714062,
0.671027521295527));
#10692=CARTESIAN_POINT('Ctrl Pts',(0.900000119565725,-1.26149151526032,
0.667969976014938));
#10693=CARTESIAN_POINT('Ctrl Pts',(0.900000124706954,-1.26425564062679,
0.664728268702146));
#10694=CARTESIAN_POINT('Ctrl Pts',(0.900000134210909,-1.26936533657602,
0.658735726205464));
#10695=CARTESIAN_POINT('Ctrl Pts',(0.900000724431276,-1.2737272220214,0.652115259198653));
#10696=CARTESIAN_POINT('Ctrl Pts',(0.900000949945503,-1.27728244659665,
0.645033014705304));
#10697=CARTESIAN_POINT('Ctrl Pts',(0.900000972753073,-1.27764200720725,
0.644316745985709));
#10698=CARTESIAN_POINT('Ctrl Pts',(0.900000992743332,-1.27799327761064,
0.64359573459864));
#10699=CARTESIAN_POINT('Ctrl Pts',(0.900001009576454,-1.27833616945273,
0.642870141642621));
#10700=CARTESIAN_POINT('Ctrl Pts',(0.900001176059944,-1.28172744954266,
0.635693858502874));
#10701=CARTESIAN_POINT('Ctrl Pts',(0.900000930108723,-1.28426399347052,
0.628153947608977));
#10702=CARTESIAN_POINT('Ctrl Pts',(0.900000539908504,-1.2858931319598,0.620419547606466));
#10703=CARTESIAN_POINT('Ctrl Pts',(0.900000289636433,-1.28693805157347,
0.615458750034127));
#10704=CARTESIAN_POINT('Ctrl Pts',(0.900000000000001,-1.28760881677759,
0.610417269724172));
#10705=CARTESIAN_POINT('Ctrl Pts',(0.900000000000001,-1.28788040985668,
0.605337476551933));
#10706=CARTESIAN_POINT('',(0.9,1.18799600975353,0.7));
#10707=CARTESIAN_POINT('',(0.9,0.696450594095222,0.7));
#10708=CARTESIAN_POINT('',(0.900000001878204,1.28788040994396,0.605337476551879));
#10709=CARTESIAN_POINT('Ctrl Pts',(0.900000000000001,1.28788040985668,0.605337476551933));
#10710=CARTESIAN_POINT('Ctrl Pts',(0.900000000000001,1.28745726486871,0.613251849878237));
#10711=CARTESIAN_POINT('Ctrl Pts',(0.900000641820462,1.28606767879774,0.621075732439556));
#10712=CARTESIAN_POINT('Ctrl Pts',(0.900000906166769,1.28379497466322,0.628648019961568));
#10713=CARTESIAN_POINT('Ctrl Pts',(0.900001053446495,1.2825287445946,0.632866896498568));
#10714=CARTESIAN_POINT('Ctrl Pts',(0.900001106693909,1.28098738700664,0.637007708770872));
#10715=CARTESIAN_POINT('Ctrl Pts',(0.900001044867119,1.27917862712792,0.641040603354488));
#10716=CARTESIAN_POINT('Ctrl Pts',(0.900000933962191,1.27593407274945,0.64827481168313));
#10717=CARTESIAN_POINT('Ctrl Pts',(0.900000399592996,1.27186725264719,0.655083885116145));
#10718=CARTESIAN_POINT('Ctrl Pts',(0.900000190596867,1.2670411556595,0.661303993035384));
#10719=CARTESIAN_POINT('Ctrl Pts',(0.900000151538061,1.26613921747962,0.662466454716044));
#10720=CARTESIAN_POINT('Ctrl Pts',(0.900000126821978,1.26521063179286,0.663608275427336));
#10721=CARTESIAN_POINT('Ctrl Pts',(0.900000125264574,1.26425564063975,0.664728268702142));
#10722=CARTESIAN_POINT('Ctrl Pts',(0.90000012217056,1.26235840892454,0.66695330163032));
#10723=CARTESIAN_POINT('Ctrl Pts',(0.900000209712012,1.26035699384613,0.66909223571964));
#10724=CARTESIAN_POINT('Ctrl Pts',(0.900000331194293,1.2582587086698,0.671141334714948));
#10725=CARTESIAN_POINT('Ctrl Pts',(0.900000660246931,1.25257519443757,0.676691620936499));
#10726=CARTESIAN_POINT('Ctrl Pts',(0.900001184896248,1.24624785575673,0.681523125886843));
#10727=CARTESIAN_POINT('Ctrl Pts',(0.900001377531805,1.23944073409582,0.685581770965975));
#10728=CARTESIAN_POINT('Ctrl Pts',(0.900001499905572,1.2351164383281,0.68816006802201));
#10729=CARTESIAN_POINT('Ctrl Pts',(0.900001510509735,1.23059756718463,0.690425789971136));
#10730=CARTESIAN_POINT('Ctrl Pts',(0.900001405318139,1.22592052877826,0.692355791713551));
#10731=CARTESIAN_POINT('Ctrl Pts',(0.900001240727996,1.21860250674997,0.695375607682216));
#10732=CARTESIAN_POINT('Ctrl Pts',(0.900000792095824,1.21098234272326,0.697541065921879));
#10733=CARTESIAN_POINT('Ctrl Pts',(0.900000425437202,1.20320741268883,0.698782789564668));
#10734=CARTESIAN_POINT('Ctrl Pts',(0.900000188792485,1.19818940410026,0.699584208982791));
#10735=CARTESIAN_POINT('Ctrl Pts',(0.900000000041206,1.19310633605572,0.699999999958324));
#10736=CARTESIAN_POINT('Ctrl Pts',(0.900000000000325,1.18799600975363,0.7));
#10737=CARTESIAN_POINT('Ctrl Pts',(0.9,1.32024227787037,0.));
#10738=CARTESIAN_POINT('Ctrl Pts',(0.9,1.31486080448354,0.100670360916234));
#10739=CARTESIAN_POINT('Ctrl Pts',(0.9,1.30947907114291,0.201341392534));
#10740=CARTESIAN_POINT('Ctrl Pts',(0.9,1.2986918099064,0.403120086121531));
#10741=CARTESIAN_POINT('Ctrl Pts',(0.900000001878204,1.29328620583358,0.504229137772713));
#10742=CARTESIAN_POINT('Ctrl Pts',(0.900000001878204,1.28788040994396,0.605337476551879));
#10743=CARTESIAN_POINT('Ctrl Pts',(0.899999999999997,-1.32024227787137,
-1.86669707469278E-11));
#10744=CARTESIAN_POINT('Ctrl Pts',(0.909148787559422,-1.30966717532842,
0.201788252636133));
#10745=CARTESIAN_POINT('Ctrl Pts',(0.91829761066914,-1.29909207410335,0.403576503749508));
#10746=CARTESIAN_POINT('Ctrl Pts',(0.92744646984625,-1.28851697422138,0.605364753299354));
#10747=CARTESIAN_POINT('Ctrl Pts',(0.699273108318574,-1.31559634352334,
-5.7001548815619E-6));
#10748=CARTESIAN_POINT('Ctrl Pts',(0.708743431409066,-1.30502123870946,
0.20178254329682));
#10749=CARTESIAN_POINT('Ctrl Pts',(0.718213789763005,-1.2944461351935,0.403570785162392));
#10750=CARTESIAN_POINT('Ctrl Pts',(0.727684183892774,-1.28387103300525,
0.605359025419352));
#10751=CARTESIAN_POINT('Ctrl Pts',(0.498558799217305,-1.31100715552056,
-1.1774619888836E-5));
#10752=CARTESIAN_POINT('Ctrl Pts',(0.508350677965937,-1.30043204942944,
0.201776459055217));
#10753=CARTESIAN_POINT('Ctrl Pts',(0.518142591787393,-1.28985694462582,
0.403564691096996));
#10754=CARTESIAN_POINT('Ctrl Pts',(0.527934541191295,-1.27928184113929,
0.60535292148228));
#10755=CARTESIAN_POINT('Ctrl Pts',(0.29785707328833,-1.3064367443434,-1.84041486642056E-5));
#10756=CARTESIAN_POINT('Ctrl Pts',(0.307970527825607,-1.29586163794,0.20176981888596));
#10757=CARTESIAN_POINT('Ctrl Pts',(0.318084017341356,-1.28528653282298,
0.403558040236175));
#10758=CARTESIAN_POINT('Ctrl Pts',(0.328197542344371,-1.27471142901691,
0.605346259877786));
#10759=CARTESIAN_POINT('',(0.32957180616905,-1.2747428754212,0.605346305703265));
#10760=CARTESIAN_POINT('Ctrl Pts',(0.297857995688647,-1.306435779838,1.57426155444895E-16));
#10761=CARTESIAN_POINT('Ctrl Pts',(0.308429283449307,-1.29587142805659,
0.201782098465301));
#10762=CARTESIAN_POINT('Ctrl Pts',(0.319000553694994,-1.28530712634462,
0.403564200350135));
#10763=CARTESIAN_POINT('Ctrl Pts',(0.329571806169048,-1.2747428754212,0.605346305703266));
#10764=CARTESIAN_POINT('Ctrl Pts',(0.32957180616905,-1.2747428754212,0.605346305703265));
#10765=CARTESIAN_POINT('Ctrl Pts',(0.519721397561595,-1.27909449722757,
0.60534313598158));
#10766=CARTESIAN_POINT('Ctrl Pts',(0.709864288600121,-1.28346276435313,
0.605340219076093));
#10767=CARTESIAN_POINT('Ctrl Pts',(0.900000001879218,-1.28788040990034,
0.605337476551906));
#10768=CARTESIAN_POINT('Ctrl Pts',(0.90231940407953,-1.18804989493878,0.7));
#10769=CARTESIAN_POINT('Ctrl Pts',(0.712166351817731,-1.18363199317816,
0.7));
#10770=CARTESIAN_POINT('Ctrl Pts',(0.522011847238247,-1.17926361631973,
0.7));
#10771=CARTESIAN_POINT('Ctrl Pts',(0.331856371369203,-1.17491202960101,
0.7));
#10772=CARTESIAN_POINT('Ctrl Pts',(0.901648075315333,-1.21694488185794,
0.7));
#10773=CARTESIAN_POINT('Ctrl Pts',(0.711500071980331,-1.21252656425213,
0.69999998041973));
#10774=CARTESIAN_POINT('Ctrl Pts',(0.521348914609444,-1.20815772874132,
0.700000022626678));
#10775=CARTESIAN_POINT('Ctrl Pts',(0.331195161244126,-1.20380556524924,
0.7));
#10776=CARTESIAN_POINT('Ctrl Pts',(0.900484091294294,-1.26704448261357,
0.676664431332699));
#10777=CARTESIAN_POINT('Ctrl Pts',(0.710344780071471,-1.26262550764723,
0.676665329845182));
#10778=CARTESIAN_POINT('Ctrl Pts',(0.520199507967113,-1.25825584722226,
0.676666267597974));
#10779=CARTESIAN_POINT('Ctrl Pts',(0.3300487189482,-1.25390275839508,0.676667306001616));
#10780=CARTESIAN_POINT('Ctrl Pts',(0.90002687589075,-1.28672371253673,0.626983665342106));
#10781=CARTESIAN_POINT('Ctrl Pts',(0.709890987426059,-1.28230548388611,
0.626985988983916));
#10782=CARTESIAN_POINT('Ctrl Pts',(0.519747959090447,-1.27793661492756,
0.626988445273931));
#10783=CARTESIAN_POINT('Ctrl Pts',(0.329598318905021,-1.27358432286302,
0.626991130804315));
#10784=CARTESIAN_POINT('Ctrl Pts',(0.900000001879218,-1.28788040990034,
0.605337476551906));
#10785=CARTESIAN_POINT('Ctrl Pts',(0.709864288600121,-1.28346276435313,
0.605340219076093));
#10786=CARTESIAN_POINT('Ctrl Pts',(0.519721397561595,-1.27909449722757,
0.60534313598158));
#10787=CARTESIAN_POINT('Ctrl Pts',(0.32957180616905,-1.2747428754212,0.605346305703265));
#10788=CARTESIAN_POINT('',(0.331856371369201,-1.17491202962433,0.7));
#10789=CARTESIAN_POINT('Origin',(0.331856371539144,-1.1749120296049,0.6));
#10790=CARTESIAN_POINT('Ctrl Pts',(0.900000000000328,-1.18799600975363,
0.7));
#10791=CARTESIAN_POINT('Ctrl Pts',(0.71062007065371,-1.18359647108512,0.7));
#10792=CARTESIAN_POINT('Ctrl Pts',(0.521238702715143,-1.17924592340069,
0.7));
#10793=CARTESIAN_POINT('Ctrl Pts',(0.331856371369203,-1.17491202960101,
0.7));
#10794=CARTESIAN_POINT('Origin',(6.87409734069396,-2.22251806091942E-16,
0.7));
#10795=CARTESIAN_POINT('',(0.331856371879032,1.17491202961268,0.7));
#10796=CARTESIAN_POINT('',(0.331856371369201,-0.75,0.7));
#10797=CARTESIAN_POINT('Ctrl Pts',(0.331856371879031,1.17491202961268,0.7));
#10798=CARTESIAN_POINT('Ctrl Pts',(0.521238703055026,1.1792459234085,0.7));
#10799=CARTESIAN_POINT('Ctrl Pts',(0.710620070823648,1.18359647108907,0.7));
#10800=CARTESIAN_POINT('Ctrl Pts',(0.900000000000325,1.18799600975363,0.7));
#10801=CARTESIAN_POINT('Ctrl Pts',(0.297857073289265,1.30643674434242,-1.84041299971672E-5));
#10802=CARTESIAN_POINT('Ctrl Pts',(0.30797052782623,1.29586163793935,0.201769818898405));
#10803=CARTESIAN_POINT('Ctrl Pts',(0.318084017341667,1.28528653282265,0.403558040242397));
#10804=CARTESIAN_POINT('Ctrl Pts',(0.328197542344371,1.27471142901691,0.605346259877786));
#10805=CARTESIAN_POINT('Ctrl Pts',(0.49855879921793,1.31100715551957,-1.17746012218085E-5));
#10806=CARTESIAN_POINT('Ctrl Pts',(0.50835067796626,1.30043204942878,0.201776459067662));
#10807=CARTESIAN_POINT('Ctrl Pts',(0.518142591787414,1.28985694462549,0.403564691103219));
#10808=CARTESIAN_POINT('Ctrl Pts',(0.527934541191015,1.27928184113928,0.60535292148228));
#10809=CARTESIAN_POINT('Ctrl Pts',(0.699273108318888,1.31559634352235,-5.70013621459206E-6));
#10810=CARTESIAN_POINT('Ctrl Pts',(0.708743431409089,1.3050212387088,0.201782543309265));
#10811=CARTESIAN_POINT('Ctrl Pts',(0.718213789762737,1.29444613519316,0.403570785168614));
#10812=CARTESIAN_POINT('Ctrl Pts',(0.727684183892215,1.28387103300524,0.605359025419352));
#10813=CARTESIAN_POINT('Ctrl Pts',(0.9,1.32024227787037,-6.93889390390723E-18));
#10814=CARTESIAN_POINT('Ctrl Pts',(0.909148787559144,1.30966717532775,0.201788252648578));
#10815=CARTESIAN_POINT('Ctrl Pts',(0.918297610668582,1.29909207410301,0.403576503755731));
#10816=CARTESIAN_POINT('Ctrl Pts',(0.927446469845411,1.28851697422136,0.605364753299355));
#10817=CARTESIAN_POINT('',(0.329571806169048,1.2747428754212,0.605346305703265));
#10818=CARTESIAN_POINT('Ctrl Pts',(0.900000001879216,1.28788040990034,0.605337476551906));
#10819=CARTESIAN_POINT('Ctrl Pts',(0.709864288600119,1.28346276435313,0.605340219076093));
#10820=CARTESIAN_POINT('Ctrl Pts',(0.519721397561593,1.27909449722757,0.60534313598158));
#10821=CARTESIAN_POINT('Ctrl Pts',(0.329571806169048,1.2747428754212,0.605346305703265));
#10822=CARTESIAN_POINT('Ctrl Pts',(0.329571806169048,1.2747428754212,0.605346305703265));
#10823=CARTESIAN_POINT('Ctrl Pts',(0.319000553694994,1.28530712634462,0.403564200350134));
#10824=CARTESIAN_POINT('Ctrl Pts',(0.308429283449307,1.29587142805659,0.201782098465301));
#10825=CARTESIAN_POINT('Ctrl Pts',(0.297857995688647,1.306435779838,6.03900610074426E-17));
#10826=CARTESIAN_POINT('Ctrl Pts',(0.331856371369201,1.17491202960101,0.7));
#10827=CARTESIAN_POINT('Ctrl Pts',(0.522011847238246,1.17926361631973,0.7));
#10828=CARTESIAN_POINT('Ctrl Pts',(0.712166351817729,1.18363199317816,0.7));
#10829=CARTESIAN_POINT('Ctrl Pts',(0.902319404079528,1.18804989493878,0.7));
#10830=CARTESIAN_POINT('Ctrl Pts',(0.331195161244124,1.20380556524924,0.7));
#10831=CARTESIAN_POINT('Ctrl Pts',(0.521348914609443,1.20815772874132,0.700000022626678));
#10832=CARTESIAN_POINT('Ctrl Pts',(0.711500071980329,1.21252656425213,0.69999998041973));
#10833=CARTESIAN_POINT('Ctrl Pts',(0.901648075315331,1.21694488185794,0.7));
#10834=CARTESIAN_POINT('Ctrl Pts',(0.330048718948197,1.25390275839508,0.676667306001616));
#10835=CARTESIAN_POINT('Ctrl Pts',(0.52019950796711,1.25825584722226,0.676666267597973));
#10836=CARTESIAN_POINT('Ctrl Pts',(0.710344780071469,1.26262550764723,0.676665329845182));
#10837=CARTESIAN_POINT('Ctrl Pts',(0.900484091294292,1.26704448261357,0.676664431332698));
#10838=CARTESIAN_POINT('Ctrl Pts',(0.329598318905018,1.27358432286302,0.626991130804315));
#10839=CARTESIAN_POINT('Ctrl Pts',(0.519747959090446,1.27793661492756,0.62698844527393));
#10840=CARTESIAN_POINT('Ctrl Pts',(0.709890987426057,1.28230548388611,0.626985988983916));
#10841=CARTESIAN_POINT('Ctrl Pts',(0.900026875890748,1.28672371253673,0.626983665342106));
#10842=CARTESIAN_POINT('Ctrl Pts',(0.329571806169048,1.2747428754212,0.605346305703265));
#10843=CARTESIAN_POINT('Ctrl Pts',(0.519721397561593,1.27909449722757,0.60534313598158));
#10844=CARTESIAN_POINT('Ctrl Pts',(0.709864288600119,1.28346276435313,0.605340219076093));
#10845=CARTESIAN_POINT('Ctrl Pts',(0.900000001879216,1.28788040990034,0.605337476551906));
#10846=CARTESIAN_POINT('Origin',(0.331856371369202,1.17491202960101,0.6));
#10847=CARTESIAN_POINT('Origin',(0.331856371369202,1.17491202960101,0.6));
#10848=CARTESIAN_POINT('Origin',(0.331856371369201,1.17491202960879,0.6));
#10849=CARTESIAN_POINT('Origin',(0.331856371369202,1.17491202960101,0.6));
#10850=CARTESIAN_POINT('Origin',(12.8681436286308,1.83274446434879,0.6));
#10851=CARTESIAN_POINT('Origin',(12.8681436286308,1.83274446434879,0.6));
#10852=CARTESIAN_POINT('',(12.9680065821063,1.83274446434879,0.605233595624294));
#10853=CARTESIAN_POINT('Origin',(12.8681436286308,1.83274446434879,0.6));
#10854=CARTESIAN_POINT('Origin',(12.8681436286308,1.83274446434879,0.6));
#10855=CARTESIAN_POINT('Origin',(0.331856371369201,-1.17491202960101,0.6));
#10856=CARTESIAN_POINT('Origin',(0.331856371369201,-1.17491202960101,0.6));
#10857=CARTESIAN_POINT('Origin',(0.331856371369201,-1.17491202960101,0.6));
#10858=CARTESIAN_POINT('Origin',(0.331856371369201,-0.75,0.6));
#10859=CARTESIAN_POINT('Ctrl Pts',(0.297750759617602,-1.30654294555098,
-0.00204689530870639));
#10860=CARTESIAN_POINT('Ctrl Pts',(0.308357792853923,-1.29594287152607,
0.200417501569666));
#10861=CARTESIAN_POINT('Ctrl Pts',(0.318964808457496,-1.28534284790734,
0.40288190189057));
#10862=CARTESIAN_POINT('Ctrl Pts',(0.329571806169048,-1.2747428754212,0.605346305703266));
#10863=CARTESIAN_POINT('Ctrl Pts',(0.268364475985512,-1.30579334864515,
-0.000546070465277405));
#10864=CARTESIAN_POINT('Ctrl Pts',(0.278972236061358,-1.29519218153762,
0.201918231169276));
#10865=CARTESIAN_POINT('Ctrl Pts',(0.289579970322816,-1.28459115545203,
0.404382541571378));
#10866=CARTESIAN_POINT('Ctrl Pts',(0.300187702091134,-1.27399007937578,
0.606846849214128));
#10867=CARTESIAN_POINT('Ctrl Pts',(0.217994620733579,-1.28028753054242,
0.000758348866131992));
#10868=CARTESIAN_POINT('Ctrl Pts',(0.228604439653725,-1.26968580576698,
0.203222517770204));
#10869=CARTESIAN_POINT('Ctrl Pts',(0.239214264875756,-1.259084092946,0.405686686833815));
#10870=CARTESIAN_POINT('Ctrl Pts',(0.24982407554016,-1.24848245399652,0.608150860486448));
#10871=CARTESIAN_POINT('Ctrl Pts',(0.200221638751335,-1.22875730734246,
-0.00100806500432267));
#10872=CARTESIAN_POINT('Ctrl Pts',(0.210832346469089,-1.21815680658782,
0.201456130081263));
#10873=CARTESIAN_POINT('Ctrl Pts',(0.221443027663539,-1.20755634130466,
0.403920328365886));
#10874=CARTESIAN_POINT('Ctrl Pts',(0.232053735729819,-1.1969559383274,0.606384528499152));
#10875=CARTESIAN_POINT('Ctrl Pts',(0.200161316008396,-1.20671181983024,
-0.00215909150772397));
#10876=CARTESIAN_POINT('Ctrl Pts',(0.21077201649647,-1.19611183845239,0.200305134857769));
#10877=CARTESIAN_POINT('Ctrl Pts',(0.221382717124246,-1.18551190812967,
0.402769363888924));
#10878=CARTESIAN_POINT('Ctrl Pts',(0.231993417893744,-1.17491202960101,
0.605233595624295));
#10879=CARTESIAN_POINT('Origin',(12.8681436286308,-1.83274446434879,0.6));
#10880=CARTESIAN_POINT('',(12.9680065821063,-1.83274446434879,0.605233595624295));
#10881=CARTESIAN_POINT('Origin',(12.8681436286308,-1.83274446434879,0.6));
#10882=CARTESIAN_POINT('Origin',(12.8681436286308,-1.83274446434879,0.6));
#10883=CARTESIAN_POINT('Origin',(12.8681436286308,1.1,0.6));
#10884=CARTESIAN_POINT('',(12.9680065821063,1.1,0.605233595624295));
#10885=CARTESIAN_POINT('Ctrl Pts',(12.9998428721614,-1.86475648739599,-0.00223900654757928));
#10886=CARTESIAN_POINT('Ctrl Pts',(12.9892307746816,-1.85408610159386,0.200251876006837));
#10887=CARTESIAN_POINT('Ctrl Pts',(12.9786186779927,-1.84341542867022,0.402742743472647));
#10888=CARTESIAN_POINT('Ctrl Pts',(12.9680065821063,-1.83274446434879,0.605233595624296));
#10889=CARTESIAN_POINT('Ctrl Pts',(12.9997989521977,-1.88070362541494,-0.00140096371806573));
#10890=CARTESIAN_POINT('Ctrl Pts',(12.9891868560404,-1.87003481788623,0.2010900171988));
#10891=CARTESIAN_POINT('Ctrl Pts',(12.9785747412344,-1.85936572080465,0.403580981971657));
#10892=CARTESIAN_POINT('Ctrl Pts',(12.967962646681,-1.84869634914788,0.606071933479074));
#10893=CARTESIAN_POINT('Ctrl Pts',(12.9919061104719,-1.91252097257855,-0.00013797468654593));
#10894=CARTESIAN_POINT('Ctrl Pts',(12.9812924311808,-1.9018552985481,0.202353118580234));
#10895=CARTESIAN_POINT('Ctrl Pts',(12.970678744243,-1.89118929884075,0.404844194499128));
#10896=CARTESIAN_POINT('Ctrl Pts',(12.9600650516023,-1.88052308923615,0.607335259545336));
#10897=CARTESIAN_POINT('Ctrl Pts',(12.9539932318948,-1.95585643963679,0.000158685530800887));
#10898=CARTESIAN_POINT('Ctrl Pts',(12.9433725220626,-1.94519261899951,0.202649549046396));
#10899=CARTESIAN_POINT('Ctrl Pts',(12.9327517623504,-1.93452853669393,0.40514039680648));
#10900=CARTESIAN_POINT('Ctrl Pts',(12.9221309734579,-1.92386419524738,0.607631230057729));
#10901=CARTESIAN_POINT('Ctrl Pts',(12.9129235702791,-1.96658826742031,-0.00142816374191492));
#10902=CARTESIAN_POINT('Ctrl Pts',(12.9022969271978,-1.95592037993921,0.201062184830579));
#10903=CARTESIAN_POINT('Ctrl Pts',(12.891670251582,-1.94525202616943,0.403552507423554));
#10904=CARTESIAN_POINT('Ctrl Pts',(12.8810434760214,-1.93458357684419,0.60604282089977));
#10905=CARTESIAN_POINT('Ctrl Pts',(12.8891437477602,-1.96405813112492,-0.00280773857265357));
#10906=CARTESIAN_POINT('Ctrl Pts',(12.8785151960038,-1.95338599020215,0.199682283294402));
#10907=CARTESIAN_POINT('Ctrl Pts',(12.8678865709412,-1.94271355010484,0.402172286243574));
#10908=CARTESIAN_POINT('Ctrl Pts',(12.8572578715866,-1.93204080633595,0.604662269998931));
#10909=CARTESIAN_POINT('Ctrl Pts',(12.9997255308004,-1.86463850151065,-4.9439619065339E-17));
#10910=CARTESIAN_POINT('Ctrl Pts',(12.9891525471135,-1.85400744222428,0.201744546927532));
#10911=CARTESIAN_POINT('Ctrl Pts',(12.9785795642115,-1.84337609791338,0.403489078876654));
#10912=CARTESIAN_POINT('Ctrl Pts',(12.9680065821063,-1.83274446434879,0.605233595624296));
#10913=CARTESIAN_POINT('Ctrl Pts',(12.8891409639924,1.96405533594058,-0.00275470357795049));
#10914=CARTESIAN_POINT('Ctrl Pts',(12.8785133401458,1.95338412669368,0.199717639954231));
#10915=CARTESIAN_POINT('Ctrl Pts',(12.8678856430057,1.9427126183241,0.402189964571813));
#10916=CARTESIAN_POINT('Ctrl Pts',(12.8572578715866,1.93204080633595,0.604662269998929));
#10917=CARTESIAN_POINT('Ctrl Pts',(12.9049941793403,1.96574209420267,-0.00183498696757459));
#10918=CARTESIAN_POINT('Ctrl Pts',(12.8943678341644,1.95507368670196,0.20063757283533));
#10919=CARTESIAN_POINT('Ctrl Pts',(12.8837414238008,1.94440496992476,0.403110113573296));
#10920=CARTESIAN_POINT('Ctrl Pts',(12.8731149412098,1.93373598667478,0.605582637266155));
#10921=CARTESIAN_POINT('Ctrl Pts',(12.9374710816243,1.9613461313261,-0.000364592700753267));
#10922=CARTESIAN_POINT('Ctrl Pts',(12.9268487371951,1.95068187676899,0.202108391447626));
#10923=CARTESIAN_POINT('Ctrl Pts',(12.9162262930262,1.94001732715406,0.404581355450702));
#10924=CARTESIAN_POINT('Ctrl Pts',(12.9056038462248,1.92935253789361,0.607054307450502));
#10925=CARTESIAN_POINT('Ctrl Pts',(12.9846523118271,1.92834870343354,0.000369250346899581));
#10926=CARTESIAN_POINT('Ctrl Pts',(12.974038022963,1.91768545846127,0.202842678583437));
#10927=CARTESIAN_POINT('Ctrl Pts',(12.9634237233674,1.90702194269714,0.405316092420461));
#10928=CARTESIAN_POINT('Ctrl Pts',(12.9528094065597,1.89635817580376,0.607789492622546));
#10929=CARTESIAN_POINT('Ctrl Pts',(12.9997742127558,1.88867440031858,-0.000928907044737527));
#10930=CARTESIAN_POINT('Ctrl Pts',(12.9891630904765,1.8780073281596,0.201544447891303));
#10931=CARTESIAN_POINT('Ctrl Pts',(12.9785517991681,1.86733992038445,0.404017776344753));
#10932=CARTESIAN_POINT('Ctrl Pts',(12.9679406789684,1.85667229154743,0.606491102406462));
#10933=CARTESIAN_POINT('Ctrl Pts',(12.9998400927033,1.86475369267134,-0.00218597132744988));
#10934=CARTESIAN_POINT('Ctrl Pts',(12.9892289217097,1.85408423839396,0.200287232817622));
#10935=CARTESIAN_POINT('Ctrl Pts',(12.9786177515068,1.84341449704483,0.402760421876702));
#10936=CARTESIAN_POINT('Ctrl Pts',(12.9680065821063,1.83274446434879,0.605233595624294));
#10937=CARTESIAN_POINT('Ctrl Pts',(12.9680065821063,1.83274446434879,0.605233595624294));
#10938=CARTESIAN_POINT('Ctrl Pts',(12.9785795642115,1.84337609791338,0.403489078876654));
#10939=CARTESIAN_POINT('Ctrl Pts',(12.9891525471135,1.85400744222428,0.201744546927532));
#10940=CARTESIAN_POINT('Ctrl Pts',(12.9997255308004,1.86463850151065,1.86916454536501E-16));
#10941=CARTESIAN_POINT('Ctrl Pts',(12.6,1.80383022254432,0.7));
#10942=CARTESIAN_POINT('Ctrl Pts',(12.6893984576578,1.8133105623702,0.7));
#10943=CARTESIAN_POINT('Ctrl Pts',(12.7787800350189,1.82294762441299,0.7));
#10944=CARTESIAN_POINT('Ctrl Pts',(12.8681436286308,1.83274446434879,0.7));
#10945=CARTESIAN_POINT('Ctrl Pts',(12.5969393303222,1.83269196733649,0.7));
#10946=CARTESIAN_POINT('Ctrl Pts',(12.686303642571,1.84217134991284,0.700000098415946));
#10947=CARTESIAN_POINT('Ctrl Pts',(12.7756511334299,1.85180730951691,0.699999896874207));
#10948=CARTESIAN_POINT('Ctrl Pts',(12.8649798835675,1.86160311979107,0.7));
#10949=CARTESIAN_POINT('Ctrl Pts',(12.5916356538948,1.88270499442536,0.67643906321291));
#10950=CARTESIAN_POINT('Ctrl Pts',(12.6809412203008,1.89218243450198,0.676434576658958));
#10951=CARTESIAN_POINT('Ctrl Pts',(12.7702288461642,1.90181652272411,0.676430055978541));
#10952=CARTESIAN_POINT('Ctrl Pts',(12.8594976525144,1.91161025179704,0.676425356750174));
#10953=CARTESIAN_POINT('Ctrl Pts',(12.58957419749,1.90214427893475,0.626447702441804));
#10954=CARTESIAN_POINT('Ctrl Pts',(12.6788572782758,1.91161594713488,0.626436135819418));
#10955=CARTESIAN_POINT('Ctrl Pts',(12.7681225846323,1.92124403769089,0.626424372515079));
#10956=CARTESIAN_POINT('Ctrl Pts',(12.8573684983393,1.93103170500986,0.626412260100396));
#10957=CARTESIAN_POINT('Ctrl Pts',(12.5894662143615,1.90316254677271,0.604704117718382));
#10958=CARTESIAN_POINT('Ctrl Pts',(12.6787484942245,1.91263121188366,0.60469048808123));
#10959=CARTESIAN_POINT('Ctrl Pts',(12.7680127446979,1.92225628370762,0.604676541242762));
#10960=CARTESIAN_POINT('Ctrl Pts',(12.8572578715866,1.93204080633595,0.60466226999893));
#10961=CARTESIAN_POINT('Ctrl Pts',(0.200160815981423,1.20671231935208,-0.00216863259073552));
#10962=CARTESIAN_POINT('Ctrl Pts',(0.21077168314515,1.19611217146534,0.200298774135678));
#10963=CARTESIAN_POINT('Ctrl Pts',(0.221382550448584,1.18551207463533,0.402766183527835));
#10964=CARTESIAN_POINT('Ctrl Pts',(0.231993417893744,1.17491202960101,0.605233595624295));
#10965=CARTESIAN_POINT('Ctrl Pts',(0.200241246305444,1.23610630273461,-0.000633930584249493));
#10966=CARTESIAN_POINT('Ctrl Pts',(0.210852138766318,1.22550544237485,0.201833432539687));
#10967=CARTESIAN_POINT('Ctrl Pts',(0.221462948692539,1.21490467236247,0.404300804744641));
#10968=CARTESIAN_POINT('Ctrl Pts',(0.232073841675177,1.20430390790287,0.60676817279077));
#10969=CARTESIAN_POINT('Ctrl Pts',(0.224595236946023,1.28704077752974,0.000756396927320467));
#10970=CARTESIAN_POINT('Ctrl Pts',(0.235204871724134,1.27643877611169,0.203223757667495));
#10971=CARTESIAN_POINT('Ctrl Pts',(0.245814524913363,1.26583679641595,0.405691118453359));
#10972=CARTESIAN_POINT('Ctrl Pts',(0.256424148042823,1.25523487973404,0.608158484046399));
#10973=CARTESIAN_POINT('Ctrl Pts',(0.275710547013829,1.30598124743532,-0.000930817763883136));
#10974=CARTESIAN_POINT('Ctrl Pts',(0.286318282165364,1.29538020346814,0.201536689442792));
#10975=CARTESIAN_POINT('Ctrl Pts',(0.296926023167072,1.2847792285374,0.404004199876323));
#10976=CARTESIAN_POINT('Ctrl Pts',(0.307533728110612,1.27417827838713,0.606471713336412));
#10977=CARTESIAN_POINT('Ctrl Pts',(0.297750259763447,1.30654344507719,-0.0020564363997533));
#10978=CARTESIAN_POINT('Ctrl Pts',(0.308357459618374,1.29594320454196,0.200411140842193));
#10979=CARTESIAN_POINT('Ctrl Pts',(0.318964641840002,1.28534301441448,0.402878721526778));
#10980=CARTESIAN_POINT('Ctrl Pts',(0.329571806169048,1.2747428754212,0.605346305703265));
#10981=CARTESIAN_POINT('Origin',(13.0002740930491,2.2,-0.0104671912485888));
#10982=CARTESIAN_POINT('Origin',(0.331856371369202,1.17491202960101,0.6));
#10983=CARTESIAN_POINT('',(0.331856371879032,1.17491202961268,0.9));
#10984=CARTESIAN_POINT('',(0.0322675109428289,1.17491202960101,0.615700786872883));
#10985=CARTESIAN_POINT('Origin',(0.331856371369201,1.17491202962433,0.6));
#10986=CARTESIAN_POINT('',(0.325002675768741,1.47440456706157,0.616038917109795));
#10987=CARTESIAN_POINT('Origin',(0.331856371369202,1.17491202960101,0.6));
#10988=CARTESIAN_POINT('Origin',(0.331856371369201,1.17491202960101,0.6));
#10989=CARTESIAN_POINT('Origin',(12.8681436286308,1.83274446434879,0.6));
#10990=CARTESIAN_POINT('',(12.8681436286308,1.83274446434879,0.9));
#10991=CARTESIAN_POINT('',(12.8354863574981,2.13063349031027,0.613986809996789));
#10992=CARTESIAN_POINT('Origin',(12.8681436286308,1.83274446434879,0.6));
#10993=CARTESIAN_POINT('',(13.1677324890572,1.83274446434879,0.615700786872883));
#10994=CARTESIAN_POINT('Origin',(12.8681436286308,1.83274446434879,0.6));
#10995=CARTESIAN_POINT('Origin',(12.8681436286308,1.83274446434879,0.6));
#10996=CARTESIAN_POINT('Origin',(0.331856371369201,-1.17491202960101,0.6));
#10997=CARTESIAN_POINT('',(0.331856371369201,-1.17491202962433,0.9));
#10998=CARTESIAN_POINT('',(0.325002675768743,-1.47440456706157,0.616038917109795));
#10999=CARTESIAN_POINT('Origin',(0.331856371879032,-1.17491202961268,0.6));
#11000=CARTESIAN_POINT('',(0.0322675109428289,-1.17491202960101,0.615700786872884));
#11001=CARTESIAN_POINT('Origin',(0.331856371369201,-1.17491202960101,0.6));
#11002=CARTESIAN_POINT('Origin',(0.331856371369201,-1.17491202960101,0.6));
#11003=CARTESIAN_POINT('Origin',(0.331856371369201,-0.75,0.6));
#11004=CARTESIAN_POINT('',(0.0322675109428289,-0.75,0.615700786872883));
#11005=CARTESIAN_POINT('',(0.331856371369201,-0.75,0.9));
#11006=CARTESIAN_POINT('Ctrl Pts',(0.292429673212981,-1.5069793045954,-0.00614074949474724));
#11007=CARTESIAN_POINT('Ctrl Pts',(0.303287396789886,-1.49612100698918,
0.201252467440773));
#11008=CARTESIAN_POINT('Ctrl Pts',(0.314145064588525,-1.48526276089333,
0.408645689616972));
#11009=CARTESIAN_POINT('Ctrl Pts',(0.325002675768741,-1.47440456706157,
0.616038917109795));
#11010=CARTESIAN_POINT('Ctrl Pts',(0.204270663953122,-1.50473074636003,
-0.00163825452108868));
#11011=CARTESIAN_POINT('Ctrl Pts',(0.215130619942527,-1.49386909866124,
0.205754670272474));
#11012=CARTESIAN_POINT('Ctrl Pts',(0.225990497234893,-1.48300775583971,
0.413147615201549));
#11013=CARTESIAN_POINT('Ctrl Pts',(0.236850363534999,-1.47214617892531,
0.620540547642382));
#11014=CARTESIAN_POINT('Ctrl Pts',(0.0531014592841718,-1.42831231122466,
0.00228331220810075));
#11015=CARTESIAN_POINT('Ctrl Pts',(0.0639677431943945,-1.41744892560022,
0.209675827753147));
#11016=CARTESIAN_POINT('Ctrl Pts',(0.0748340498672138,-1.40658548887187,
0.417068339030394));
#11017=CARTESIAN_POINT('Ctrl Pts',(0.0857003072238147,-1.3957221574093,
0.624460858243749));
#11018=CARTESIAN_POINT('Ctrl Pts',(-0.000158492362241063,-1.27362248439808,
-0.0030242144278773));
#11019=CARTESIAN_POINT('Ctrl Pts',(0.0107105192099893,-1.2627628846508,
0.204368383073371));
#11020=CARTESIAN_POINT('Ctrl Pts',(0.0215794523842628,-1.25190326350425,
0.411760983371354));
#11021=CARTESIAN_POINT('Ctrl Pts',(0.0324484644510542,-1.24104375578019,
0.619153585497454));
#11022=CARTESIAN_POINT('Ctrl Pts',(-0.000339460947516079,-1.20748590713937,
-0.00647730073969574));
#11023=CARTESIAN_POINT('Ctrl Pts',(0.0105295295353408,-1.19662789414299,
0.200915392321314));
#11024=CARTESIAN_POINT('Ctrl Pts',(0.0213985201647323,-1.18576993469886,
0.408308088178364));
#11025=CARTESIAN_POINT('Ctrl Pts',(0.032267510942829,-1.17491202960101,
0.615700786872884));
#11026=CARTESIAN_POINT('Ctrl Pts',(0.292751161823634,-1.50665779898694,
4.33680868994202E-17));
#11027=CARTESIAN_POINT('Ctrl Pts',(0.30350172143464,-1.49590667092872,0.205346300540216));
#11028=CARTESIAN_POINT('Ctrl Pts',(0.314252226354851,-1.48515559337638,
0.410692606218909));
#11029=CARTESIAN_POINT('Ctrl Pts',(0.325002675768741,-1.47440456706157,
0.616038917109795));
#11030=CARTESIAN_POINT('Ctrl Pts',(0.032267510942829,-1.17491202960101,
0.615700786872884));
#11031=CARTESIAN_POINT('Ctrl Pts',(0.021511673816962,-1.18565689645617,
0.410467188483275));
#11032=CARTESIAN_POINT('Ctrl Pts',(0.0107558368367201,-1.19640181653194,
0.205233592872363));
#11033=CARTESIAN_POINT('Ctrl Pts',(-2.19605150036939E-16,-1.20714678905882,
1.11889664200504E-16));
#11034=CARTESIAN_POINT('Origin',(12.8681436286308,-1.83274446434879,0.6));
#11035=CARTESIAN_POINT('',(13.1677324890572,-1.83274446434879,0.615700786872883));
#11036=CARTESIAN_POINT('',(12.8354863574981,-2.13063349031027,0.613986809996789));
#11037=CARTESIAN_POINT('Origin',(12.8681436286308,-1.83274446434879,0.6));
#11038=CARTESIAN_POINT('',(12.8681436286308,-1.83274446434879,0.9));
#11039=CARTESIAN_POINT('Origin',(12.8681436286308,-1.83274446434879,0.6));
#11040=CARTESIAN_POINT('Origin',(12.8681436286308,-1.83274446434879,0.6));
#11041=CARTESIAN_POINT('Origin',(12.8681436286308,1.1,0.6));
#11042=CARTESIAN_POINT('',(13.1677324890572,1.1,0.615700786872883));
#11043=CARTESIAN_POINT('',(12.8681436286308,1.1,0.9));
#11044=CARTESIAN_POINT('Ctrl Pts',(12.8681436286308,-1.83274446434879,0.9));
#11045=CARTESIAN_POINT('Ctrl Pts',(11.0848390724976,-1.63724259846481,0.9));
#11046=CARTESIAN_POINT('Ctrl Pts',(6.90843812479705,-1.33014681916253,0.9));
#11047=CARTESIAN_POINT('Ctrl Pts',(2.72316671642812,-1.22963564084767,0.9));
#11048=CARTESIAN_POINT('Ctrl Pts',(0.331856371369203,-1.17491202960101,
0.9));
#11049=CARTESIAN_POINT('Ctrl Pts',(12.8586523934408,-1.91932043067563,0.9));
#11050=CARTESIAN_POINT('Ctrl Pts',(11.0774332085042,-1.7238803779394,0.89999435405169));
#11051=CARTESIAN_POINT('Ctrl Pts',(6.90489492800773,-1.41683381760594,0.900002805573959));
#11052=CARTESIAN_POINT('Ctrl Pts',(2.72111811994416,-1.31633797570969,0.90000078069347));
#11053=CARTESIAN_POINT('Ctrl Pts',(0.329872740993971,-1.26159263654569,
0.9));
#11054=CARTESIAN_POINT('Ctrl Pts',(12.8422006781022,-2.06938763738452,0.829321796184829));
#11055=CARTESIAN_POINT('Ctrl Pts',(11.0645720435655,-1.87407163985848,0.829602081442736));
#11056=CARTESIAN_POINT('Ctrl Pts',(6.89876476423634,-1.56711486110062,0.829953500700133));
#11057=CARTESIAN_POINT('Ctrl Pts',(2.71756729604702,-1.46664725828863,0.829952661937692));
#11058=CARTESIAN_POINT('Ctrl Pts',(0.326433810179884,-1.41186690836963,
0.829991693349937));
#11059=CARTESIAN_POINT('Ctrl Pts',(12.8358182377562,-2.12760618633201,0.679236780301187));
#11060=CARTESIAN_POINT('Ctrl Pts',(11.0595580661442,-1.93265366192027,0.679962478070753));
#11061=CARTESIAN_POINT('Ctrl Pts',(6.89634818471837,-1.62613750062048,0.680874066334139));
#11062=CARTESIAN_POINT('Ctrl Pts',(2.71617242066404,-1.52567909229178,0.680871998075852));
#11063=CARTESIAN_POINT('Ctrl Pts',(0.325082213976654,-1.47092890938704,
0.680973392412944));
#11064=CARTESIAN_POINT('Ctrl Pts',(12.8354863574981,-2.13063349031027,0.613986809996789));
#11065=CARTESIAN_POINT('Ctrl Pts',(11.0592740266891,-1.93586902238569,0.614841183901826));
#11066=CARTESIAN_POINT('Ctrl Pts',(6.89620783868867,-1.62958780289117,0.615922665333222));
#11067=CARTESIAN_POINT('Ctrl Pts',(2.71609101918193,-1.52912950204849,0.615919334096661));
#11068=CARTESIAN_POINT('Ctrl Pts',(0.325002675768742,-1.47440456706157,
0.616038917109795));
#11069=CARTESIAN_POINT('Ctrl Pts',(0.325002675768742,-1.47440456706157,
0.616038917109795));
#11070=CARTESIAN_POINT('Ctrl Pts',(2.71609101918193,-1.52912950204849,0.615919334096661));
#11071=CARTESIAN_POINT('Ctrl Pts',(6.89620783868867,-1.62958780289117,0.615922665333222));
#11072=CARTESIAN_POINT('Ctrl Pts',(11.0592740266891,-1.93586902238569,0.614841183901826));
#11073=CARTESIAN_POINT('Ctrl Pts',(12.8354863574981,-2.13063349031027,0.613986809996789));
#11074=CARTESIAN_POINT('Ctrl Pts',(12.8681436286308,-1.83274446434879,0.9));
#11075=CARTESIAN_POINT('Ctrl Pts',(11.0848390724976,-1.63724259846481,0.9));
#11076=CARTESIAN_POINT('Ctrl Pts',(6.90843812479705,-1.33014681916253,0.9));
#11077=CARTESIAN_POINT('Ctrl Pts',(2.72316671642812,-1.22963564084767,0.9));
#11078=CARTESIAN_POINT('Ctrl Pts',(0.331856371369203,-1.17491202960101,
0.9));
#11079=CARTESIAN_POINT('Ctrl Pts',(13.2003520234216,-1.86554403325358,-0.00671700702553119));
#11080=CARTESIAN_POINT('Ctrl Pts',(13.1894788444661,-1.85461114646479,0.200755606855839));
#11081=CARTESIAN_POINT('Ctrl Pts',(13.1786056663403,-1.84367795836273,0.40822820490283));
#11082=CARTESIAN_POINT('Ctrl Pts',(13.1677324890572,-1.83274446434879,0.615700786872884));
#11083=CARTESIAN_POINT('Ctrl Pts',(13.200220264666,-1.91338509859121,-0.00420290020003313));
#11084=CARTESIAN_POINT('Ctrl Pts',(13.1893470894366,-1.90245705934317,0.203270015787334));
#11085=CARTESIAN_POINT('Ctrl Pts',(13.1784738563058,-1.89152871992859,0.410742913234898));
#11086=CARTESIAN_POINT('Ctrl Pts',(13.1676006827814,-1.88060011874606,0.61821580043722));
#11087=CARTESIAN_POINT('Ctrl Pts',(13.1765676699515,-2.00888806967359,-0.000409897060868941));
#11088=CARTESIAN_POINT('Ctrl Pts',(13.1656896254949,-1.99796966505382,0.207063364242462));
#11089=CARTESIAN_POINT('Ctrl Pts',(13.1548115799789,-1.98705090404177,0.414536607525659));
#11090=CARTESIAN_POINT('Ctrl Pts',(13.1439334900924,-1.97613202744891,0.622009843787749));
#11091=CARTESIAN_POINT('Ctrl Pts',(13.0627995670833,-2.13884429305335,0.000475886042502645));
#11092=CARTESIAN_POINT('Ctrl Pts',(13.0518999280859,-2.12793157960824,0.207948441605934));
#11093=CARTESIAN_POINT('Ctrl Pts',(13.041000104914,-2.11701865581933,0.415420978499924));
#11094=CARTESIAN_POINT('Ctrl Pts',(13.0301002136907,-2.10610551685206,0.62289350259018));
#11095=CARTESIAN_POINT('Ctrl Pts',(12.9395973356642,-2.17103883395928,-0.00428435975826336));
#11096=CARTESIAN_POINT('Ctrl Pts',(12.9286794517625,-2.16011362679945,0.203186612960554));
#11097=CARTESIAN_POINT('Ctrl Pts',(12.9177614752639,-2.14918756369419,0.410657536673191));
#11098=CARTESIAN_POINT('Ctrl Pts',(12.9068431708026,-2.13826180183499,0.618128462699307));
#11099=CARTESIAN_POINT('Ctrl Pts',(12.8682582931239,-2.16344935299393,-0.00842301254802964));
#11100=CARTESIAN_POINT('Ctrl Pts',(12.857334548107,-2.15251107312608,0.1990469563258));
#11101=CARTESIAN_POINT('Ctrl Pts',(12.8464105706338,-2.1415724540018,0.406516897309109));
#11102=CARTESIAN_POINT('Ctrl Pts',(12.8354863574981,-2.13063349031027,0.61398680999679));
#11103=CARTESIAN_POINT('Ctrl Pts',(13.2,-1.86519007666192,-2.60208521396521E-17));
#11104=CARTESIAN_POINT('Ctrl Pts',(13.1892441622028,-1.85437516893481,0.20523361119958));
#11105=CARTESIAN_POINT('Ctrl Pts',(13.1784883252177,-1.84355996631422,0.410467206902138));
#11106=CARTESIAN_POINT('Ctrl Pts',(13.1677324890572,-1.83274446434879,0.615700786872884));
#11107=CARTESIAN_POINT('Ctrl Pts',(12.8354863574981,-2.13063349031027,0.61398680999679));
#11108=CARTESIAN_POINT('Ctrl Pts',(12.8462627343229,-2.14142441807303,0.409324567403199));
#11109=CARTESIAN_POINT('Ctrl Pts',(12.8570388818204,-2.15221501053143,0.204662297274642));
#11110=CARTESIAN_POINT('Ctrl Pts',(12.8678148030684,-2.16300527278357,2.15973072759112E-16));
#11111=CARTESIAN_POINT('Ctrl Pts',(12.868249917342,2.16344096606744,-0.0082639349430893));
#11112=CARTESIAN_POINT('Ctrl Pts',(12.8573289641336,2.15250548166836,0.19915300804817));
#11113=CARTESIAN_POINT('Ctrl Pts',(12.8464077785869,2.14156965818488,0.406569923163064));
#11114=CARTESIAN_POINT('Ctrl Pts',(12.8354863574981,2.13063349031027,0.613986809996789));
#11115=CARTESIAN_POINT('Ctrl Pts',(12.9158092820513,2.16850062662823,-0.00550483257449158));
#11116=CARTESIAN_POINT('Ctrl Pts',(12.9048922561706,2.15757374897544,0.201912774743134));
#11117=CARTESIAN_POINT('Ctrl Pts',(12.8939750281693,2.14664650750606,0.409330354360154));
#11118=CARTESIAN_POINT('Ctrl Pts',(12.8830575663678,2.13571903132675,0.616747911798467));
#11119=CARTESIAN_POINT('Ctrl Pts',(13.0132876381743,2.15534286385676,-0.00108956416640176));
#11120=CARTESIAN_POINT('Ctrl Pts',(13.002382910411,2.14442874534411,0.206329347217122));
#11121=CARTESIAN_POINT('Ctrl Pts',(12.9914779109393,2.13351435475356,0.413748232116966));
#11122=CARTESIAN_POINT('Ctrl Pts',(12.9805728576194,2.12259976690609,0.621167106093357));
#11123=CARTESIAN_POINT('Ctrl Pts',(13.1547834649542,2.05631410774027,0.001107541479323));
#11124=CARTESIAN_POINT('Ctrl Pts',(13.1439034803964,2.04540309863889,0.208527817346591));
#11125=CARTESIAN_POINT('Ctrl Pts',(13.1330234810862,2.03449182132921,0.415948079627069));
#11126=CARTESIAN_POINT('Ctrl Pts',(13.1221434051731,2.0235803832085,0.623368331037722));
#11127=CARTESIAN_POINT('Ctrl Pts',(13.2001460482598,1.93729725403583,-0.00278676680844524));
#11128=CARTESIAN_POINT('Ctrl Pts',(13.1892758011844,1.92637447722781,0.204633283810596));
#11129=CARTESIAN_POINT('Ctrl Pts',(13.1784050234814,1.91545126126866,0.412053283701094));
#11130=CARTESIAN_POINT('Ctrl Pts',(13.1675347796435,1.9045279459447,0.619473307219386));
#11131=CARTESIAN_POINT('Ctrl Pts',(13.2003436864113,1.86553565046225,-0.00655792739252892));
#11132=CARTESIAN_POINT('Ctrl Pts',(13.1894732864596,1.85460555778322,0.200861659936414));
#11133=CARTESIAN_POINT('Ctrl Pts',(13.1786028873373,1.84367516394377,0.408281231439009));
#11134=CARTESIAN_POINT('Ctrl Pts',(13.1677324890572,1.83274446434879,0.615700786872883));
#11135=CARTESIAN_POINT('Ctrl Pts',(12.8678148030684,2.16300527278357,-3.77302356024956E-17));
#11136=CARTESIAN_POINT('Ctrl Pts',(12.8570388818204,2.15221501053142,0.204662297274639));
#11137=CARTESIAN_POINT('Ctrl Pts',(12.8462627343229,2.14142441807303,0.409324567403198));
#11138=CARTESIAN_POINT('Ctrl Pts',(12.8354863574981,2.13063349031027,0.613986809996789));
#11139=CARTESIAN_POINT('Ctrl Pts',(13.1677324890572,1.83274446434879,0.615700786872883));
#11140=CARTESIAN_POINT('Ctrl Pts',(13.1784883252177,1.84355996631422,0.410467206902138));
#11141=CARTESIAN_POINT('Ctrl Pts',(13.1892441622028,1.85437516893481,0.20523361119958));
#11142=CARTESIAN_POINT('Ctrl Pts',(13.2,1.86519007666192,9.4542429440736E-17));
#11143=CARTESIAN_POINT('Ctrl Pts',(0.3318563713692,1.17491202960101,0.9));
#11144=CARTESIAN_POINT('Ctrl Pts',(2.72316671642811,1.22963564084767,0.9));
#11145=CARTESIAN_POINT('Ctrl Pts',(6.90843812479704,1.33014681916253,0.9));
#11146=CARTESIAN_POINT('Ctrl Pts',(11.0848390724976,1.63724259846481,0.9));
#11147=CARTESIAN_POINT('Ctrl Pts',(12.8681436286308,1.83274446434879,0.9));
#11148=CARTESIAN_POINT('Ctrl Pts',(0.329872740993969,1.26159263654569,0.9));
#11149=CARTESIAN_POINT('Ctrl Pts',(2.72111811994415,1.31633797570969,0.90000078069347));
#11150=CARTESIAN_POINT('Ctrl Pts',(6.90489492800774,1.41683381760594,0.90000280557396));
#11151=CARTESIAN_POINT('Ctrl Pts',(11.0774332085042,1.7238803779394,0.89999435405169));
#11152=CARTESIAN_POINT('Ctrl Pts',(12.8586523934408,1.91932043067563,0.9));
#11153=CARTESIAN_POINT('Ctrl Pts',(0.326433810179882,1.41186690836963,0.829991693349937));
#11154=CARTESIAN_POINT('Ctrl Pts',(2.71756729604703,1.46664725828863,0.829952661937692));
#11155=CARTESIAN_POINT('Ctrl Pts',(6.89876476423633,1.56711486110062,0.829953500700133));
#11156=CARTESIAN_POINT('Ctrl Pts',(11.0645720435655,1.87407163985848,0.829602081442736));
#11157=CARTESIAN_POINT('Ctrl Pts',(12.8422006781022,2.06938763738452,0.829321796184828));
#11158=CARTESIAN_POINT('Ctrl Pts',(0.325082213976652,1.47092890938703,0.680973392412944));
#11159=CARTESIAN_POINT('Ctrl Pts',(2.71617242066403,1.52567909229178,0.680871998075852));
#11160=CARTESIAN_POINT('Ctrl Pts',(6.89634818471838,1.62613750062048,0.680874066334139));
#11161=CARTESIAN_POINT('Ctrl Pts',(11.0595580661442,1.93265366192027,0.679962478070753));
#11162=CARTESIAN_POINT('Ctrl Pts',(12.8358182377562,2.12760618633201,0.679236780301187));
#11163=CARTESIAN_POINT('Ctrl Pts',(0.32500267576874,1.47440456706157,0.616038917109795));
#11164=CARTESIAN_POINT('Ctrl Pts',(2.71609101918192,1.52912950204849,0.615919334096661));
#11165=CARTESIAN_POINT('Ctrl Pts',(6.89620783868868,1.62958780289117,0.615922665333222));
#11166=CARTESIAN_POINT('Ctrl Pts',(11.0592740266891,1.93586902238569,0.614841183901826));
#11167=CARTESIAN_POINT('Ctrl Pts',(12.8354863574981,2.13063349031027,0.613986809996789));
#11168=CARTESIAN_POINT('Ctrl Pts',(12.8354863574981,2.13063349031027,0.613986809996789));
#11169=CARTESIAN_POINT('Ctrl Pts',(11.0592740266891,1.93586902238569,0.614841183901826));
#11170=CARTESIAN_POINT('Ctrl Pts',(6.89620783868868,1.62958780289117,0.615922665333222));
#11171=CARTESIAN_POINT('Ctrl Pts',(2.71609101918192,1.52912950204849,0.615919334096661));
#11172=CARTESIAN_POINT('Ctrl Pts',(0.32500267576874,1.47440456706157,0.616038917109795));
#11173=CARTESIAN_POINT('Ctrl Pts',(0.331856371879031,1.17491202961268,0.900000000000001));
#11174=CARTESIAN_POINT('Ctrl Pts',(2.72316671676804,1.22963564085583,0.9));
#11175=CARTESIAN_POINT('Ctrl Pts',(6.90843812496665,1.330146819175,0.9));
#11176=CARTESIAN_POINT('Ctrl Pts',(11.0848390724976,1.63724259846481,0.9));
#11177=CARTESIAN_POINT('Ctrl Pts',(12.8681436286308,1.83274446434879,0.9));
#11178=CARTESIAN_POINT('Ctrl Pts',(-0.00034095850043725,1.20748740317979,
-0.0065058757516861));
#11179=CARTESIAN_POINT('Ctrl Pts',(0.0105285311667133,1.19662889149835,
0.200896342313063));
#11180=CARTESIAN_POINT('Ctrl Pts',(0.0213980209804115,1.18577043337405,
0.408298563174108));
#11181=CARTESIAN_POINT('Ctrl Pts',(0.0322675109428289,1.17491202960101,
0.615700786872884));
#11182=CARTESIAN_POINT('Ctrl Pts',(-9.96670524854573E-5,1.295669506487,
-0.00190176065173685));
#11183=CARTESIAN_POINT('Ctrl Pts',(0.0107698931059531,1.28480880908357,
0.205500324005663));
#11184=CARTESIAN_POINT('Ctrl Pts',(0.0216392211477595,1.27394827585187,
0.412902429485043));
#11185=CARTESIAN_POINT('Ctrl Pts',(0.0325087822871292,1.26308766450658,
0.62030451837231));
#11186=CARTESIAN_POINT('Ctrl Pts',(0.0728623575603101,1.44853010213391,
0.00227745497540766));
#11187=CARTESIAN_POINT('Ctrl Pts',(0.0837280751164453,1.43766588856392,
0.209679530627308));
#11188=CARTESIAN_POINT('Ctrl Pts',(0.0945938325013454,1.42680163888532,
0.41708160190494));
#11189=CARTESIAN_POINT('Ctrl Pts',(0.105459512942901,1.41593747613444,0.624483681552028));
#11190=CARTESIAN_POINT('Ctrl Pts',(0.226308920038025,1.50529438233544,-0.00279245331904538));
#11191=CARTESIAN_POINT('Ctrl Pts',(0.237168779176494,1.4944331215396,0.204610074087555));
#11192=CARTESIAN_POINT('Ctrl Pts',(0.248028678199983,1.48357195724705,0.412012604182119));
#11193=CARTESIAN_POINT('Ctrl Pts',(0.258888441593434,1.47271077595937,0.619415140009235));
#11194=CARTESIAN_POINT('Ctrl Pts',(0.292428177212438,1.50698080067503,-0.00616932457891824));
#11195=CARTESIAN_POINT('Ctrl Pts',(0.303286399461314,1.49612200437087,0.201233417384176));
#11196=CARTESIAN_POINT('Ctrl Pts',(0.314144565926839,1.48526325958177,0.408636164588429));
#11197=CARTESIAN_POINT('Ctrl Pts',(0.325002675768741,1.47440456706157,0.616038917109795));
#11198=CARTESIAN_POINT('Ctrl Pts',(1.62630325872826E-19,1.20714678905882,
-9.93129189996722E-17));
#11199=CARTESIAN_POINT('Ctrl Pts',(0.0107558368367203,1.19640181653194,
0.205233592872363));
#11200=CARTESIAN_POINT('Ctrl Pts',(0.0215116738169619,1.18565689645617,
0.410467188483274));
#11201=CARTESIAN_POINT('Ctrl Pts',(0.0322675109428289,1.17491202960101,
0.615700786872884));
#11202=CARTESIAN_POINT('Ctrl Pts',(0.325002675768741,1.47440456706157,0.616038917109795));
#11203=CARTESIAN_POINT('Ctrl Pts',(0.314252226354851,1.48515559337638,0.410692606218907));
#11204=CARTESIAN_POINT('Ctrl Pts',(0.30350172143464,1.49590667092872,0.205346300540215));
#11205=CARTESIAN_POINT('Ctrl Pts',(0.292751161823635,1.50665779898694,-1.27502175484295E-16));
#11206=CARTESIAN_POINT('Ctrl Pts',(12.8678148030684,-2.16300527278356,0.));
#11207=CARTESIAN_POINT('Ctrl Pts',(12.8575947095063,-2.15224352891768,0.205346305703265));
#11208=CARTESIAN_POINT('Ctrl Pts',(12.8473746159443,-2.14148178505179,0.41069261140653));
#11209=CARTESIAN_POINT('Ctrl Pts',(12.8371545223823,-2.13072004118591,0.616038917109795));
#11210=CARTESIAN_POINT('Ctrl Pts',(8.67612692265345,-1.70561506876628,0.));
#11211=CARTESIAN_POINT('Ctrl Pts',(8.67274165808153,-1.69485332490039,0.205346305703265));
#11212=CARTESIAN_POINT('Ctrl Pts',(8.66935639350961,-1.68409158103451,0.41069261140653));
#11213=CARTESIAN_POINT('Ctrl Pts',(8.6659711289377,-1.67332983716862,0.616038917109795));
#11214=CARTESIAN_POINT('Ctrl Pts',(4.48443904223854,-1.60211086545473,0.));
#11215=CARTESIAN_POINT('Ctrl Pts',(4.48788860665674,-1.59134912158884,0.205346305703265));
#11216=CARTESIAN_POINT('Ctrl Pts',(4.49133817107494,-1.58058737772296,0.41069261140653));
#11217=CARTESIAN_POINT('Ctrl Pts',(4.49478773549313,-1.56982563385707,0.616038917109795));
#11218=CARTESIAN_POINT('Ctrl Pts',(0.292751161823634,-1.50665779898694,
0.));
#11219=CARTESIAN_POINT('Ctrl Pts',(0.303035555231945,-1.49589605512106,
0.205346305703265));
#11220=CARTESIAN_POINT('Ctrl Pts',(0.313319948640256,-1.48513431125517,
0.41069261140653));
#11221=CARTESIAN_POINT('Ctrl Pts',(0.323604342048567,-1.47437256738929,
0.616038917109795));
#11222=CARTESIAN_POINT('Origin',(0.,-1.5,0.));
#11223=CARTESIAN_POINT('Origin',(6.87409734069396,-2.22044604925031E-16,
0.9));
#11224=CARTESIAN_POINT('Ctrl Pts',(0.292751161823634,1.50665779898694,0.));
#11225=CARTESIAN_POINT('Ctrl Pts',(0.303035555231945,1.49589605512106,0.205346305703265));
#11226=CARTESIAN_POINT('Ctrl Pts',(0.313319948640256,1.48513431125517,0.41069261140653));
#11227=CARTESIAN_POINT('Ctrl Pts',(0.323604342048567,1.47437256738929,0.616038917109795));
#11228=CARTESIAN_POINT('Ctrl Pts',(4.48443904223854,1.60211086545473,0.));
#11229=CARTESIAN_POINT('Ctrl Pts',(4.48788860665674,1.59134912158884,0.205346305703265));
#11230=CARTESIAN_POINT('Ctrl Pts',(4.49133817107493,1.58058737772296,0.41069261140653));
#11231=CARTESIAN_POINT('Ctrl Pts',(4.49478773549313,1.56982563385707,0.616038917109795));
#11232=CARTESIAN_POINT('Ctrl Pts',(8.67612692265345,1.70561506876628,0.));
#11233=CARTESIAN_POINT('Ctrl Pts',(8.67274165808153,1.69485332490039,0.205346305703265));
#11234=CARTESIAN_POINT('Ctrl Pts',(8.66935639350961,1.68409158103451,0.41069261140653));
#11235=CARTESIAN_POINT('Ctrl Pts',(8.66597112893769,1.67332983716862,0.616038917109795));
#11236=CARTESIAN_POINT('Ctrl Pts',(12.8678148030684,2.16300527278356,0.));
#11237=CARTESIAN_POINT('Ctrl Pts',(12.8575947095063,2.15224352891768,0.205346305703265));
#11238=CARTESIAN_POINT('Ctrl Pts',(12.8473746159443,2.14148178505179,0.41069261140653));
#11239=CARTESIAN_POINT('Ctrl Pts',(12.8371545223823,2.13072004118591,0.616038917109795));
#11240=CARTESIAN_POINT('Origin',(13.2,2.2,0.));
#11241=CARTESIAN_POINT('',(0.,0.,0.));
#11242=CARTESIAN_POINT('Origin',(6.87409734069396,-2.22251806091942E-16,
0.7));
#11243=CARTESIAN_POINT('',(3.31825992066485,1.2493322588334,0.7));
#11244=CARTESIAN_POINT('',(4.3,1.27917501057225,0.7));
#11245=CARTESIAN_POINT('Ctrl Pts',(3.31826243508713,1.24933270901874,0.7));
#11246=CARTESIAN_POINT('Ctrl Pts',(3.64552542112514,1.25866821321074,0.7));
#11247=CARTESIAN_POINT('Ctrl Pts',(3.97277304530853,1.26856018917077,0.7));
#11248=CARTESIAN_POINT('Ctrl Pts',(4.30000000005992,1.27917501058303,0.7));
#11249=CARTESIAN_POINT('',(4.3,-1.27917501057184,0.7));
#11250=CARTESIAN_POINT('',(4.3,0.742407407407408,0.7));
#11251=CARTESIAN_POINT('',(3.31825992075695,-1.24933225883136,0.7));
#11252=CARTESIAN_POINT('Ctrl Pts',(4.3000000000599,-1.27917501058303,0.7));
#11253=CARTESIAN_POINT('Ctrl Pts',(3.97277304533917,-1.26856018917177,0.7));
#11254=CARTESIAN_POINT('Ctrl Pts',(3.64552542118644,-1.25866821321259,0.7));
#11255=CARTESIAN_POINT('Ctrl Pts',(3.3182624351791,-1.24933270902137,0.7));
#11256=CARTESIAN_POINT('',(3.26759951430388,-1.24789152572578,0.7));
#11257=CARTESIAN_POINT('Ctrl Pts',(3.26760216044043,-1.24789199949781,0.7));
#11258=CARTESIAN_POINT('Ctrl Pts',(3.27154046708102,-1.24840675231115,0.699999999449966));
#11259=CARTESIAN_POINT('Ctrl Pts',(3.27549053112987,-1.2488275353013,0.699997549264952));
#11260=CARTESIAN_POINT('Ctrl Pts',(3.27944900419773,-1.24915404112413,0.699995443099811));
#11261=CARTESIAN_POINT('Ctrl Pts',(3.28202272903949,-1.24936632907779,0.699994073710794));
#11262=CARTESIAN_POINT('Ctrl Pts',(3.28459959180148,-1.24953872742098,0.699992815093061));
#11263=CARTESIAN_POINT('Ctrl Pts',(3.28717866899733,-1.24967118132558,0.699992046536556));
#11264=CARTESIAN_POINT('Ctrl Pts',(3.28888409507617,-1.24975876704947,0.699991538325205));
#11265=CARTESIAN_POINT('Ctrl Pts',(3.29059037034979,-1.2498288805585,0.699991238158591));
#11266=CARTESIAN_POINT('Ctrl Pts',(3.29229723346923,-1.24988151179005,0.69999118215758));
#11267=CARTESIAN_POINT('Ctrl Pts',(3.29393274317941,-1.24993194283473,0.699991128497625));
#11268=CARTESIAN_POINT('Ctrl Pts',(3.29556870469678,-1.24996631998408,0.699991298652463));
#11269=CARTESIAN_POINT('Ctrl Pts',(3.29720488848534,-1.24998463806557,0.699991673963628));
#11270=CARTESIAN_POINT('Ctrl Pts',(3.29943508678369,-1.25000960650399,0.699992185531049));
#11271=CARTESIAN_POINT('Ctrl Pts',(3.30166551218918,-1.25000473681137,0.699993084765318));
#11272=CARTESIAN_POINT('Ctrl Pts',(3.30389557412726,-1.24997002667259,0.699994176731177));
#11273=CARTESIAN_POINT('Ctrl Pts',(3.30868977915254,-1.24989540653807,0.699996524248132));
#11274=CARTESIAN_POINT('Ctrl Pts',(3.31348068594496,-1.24968290539118,0.699999999312134));
#11275=CARTESIAN_POINT('Ctrl Pts',(3.3182624351791,-1.24933270902137,0.7));
#11276=CARTESIAN_POINT('',(1.1,-1.19266190204492,0.7));
#11277=CARTESIAN_POINT('Ctrl Pts',(3.26760216044045,-1.24789199949781,0.7));
#11278=CARTESIAN_POINT('Ctrl Pts',(2.54512260523322,-1.2274084473838,0.7));
#11279=CARTESIAN_POINT('Ctrl Pts',(1.82256951666701,-1.20959509718369,0.7));
#11280=CARTESIAN_POINT('Ctrl Pts',(1.09999999999999,-1.19266190204553,0.7));
#11281=CARTESIAN_POINT('',(1.1,1.19266190204492,0.7));
#11282=CARTESIAN_POINT('',(1.1,-0.696450594095222,0.7));
#11283=CARTESIAN_POINT('',(3.26759952419083,1.24789152650872,0.7));
#11284=CARTESIAN_POINT('Ctrl Pts',(1.09999999999999,1.19266190204553,0.7));
#11285=CARTESIAN_POINT('Ctrl Pts',(1.82256951996781,1.20959509726105,0.7));
#11286=CARTESIAN_POINT('Ctrl Pts',(2.54512261183467,1.22740844754655,0.7));
#11287=CARTESIAN_POINT('Ctrl Pts',(3.26760217034162,1.24789199977852,0.7));
#11288=CARTESIAN_POINT('Ctrl Pts',(3.3182624351791,1.24933270902137,0.7));
#11289=CARTESIAN_POINT('Ctrl Pts',(3.3143012451848,1.2496228108833,0.699999999430174));
#11290=CARTESIAN_POINT('Ctrl Pts',(3.31033365565543,1.24981842655856,0.699997549220164));
#11291=CARTESIAN_POINT('Ctrl Pts',(3.30636302717881,1.24991943948955,0.699995443052606));
#11292=CARTESIAN_POINT('Ctrl Pts',(3.30378139908369,1.24998511620097,0.699994073661998));
#11293=CARTESIAN_POINT('Ctrl Pts',(3.3011989045204,1.25001078941611,0.699992815050698));
#11294=CARTESIAN_POINT('Ctrl Pts',(3.29861646861803,1.2499964568765,0.699992046505716));
#11295=CARTESIAN_POINT('Ctrl Pts',(3.2969088217217,1.24998697942277,0.699991538302026));
#11296=CARTESIAN_POINT('Ctrl Pts',(3.29520131971864,1.24996000972381,0.699991238145114));
#11297=CARTESIAN_POINT('Ctrl Pts',(3.29349422410899,1.24991555258537,0.699991182154076));
#11298=CARTESIAN_POINT('Ctrl Pts',(3.29185849176351,1.24987295392896,0.699991128503682));
#11299=CARTESIAN_POINT('Ctrl Pts',(3.29022322047391,1.2498143016413,0.699991298668259));
#11300=CARTESIAN_POINT('Ctrl Pts',(3.28858863969825,1.2497396036024,0.699991673987721));
#11301=CARTESIAN_POINT('Ctrl Pts',(3.286360626573,1.24963778654105,0.699992185566407));
#11302=CARTESIAN_POINT('Ctrl Pts',(3.28413408201674,1.24950616665997,0.699993084809042));
#11303=CARTESIAN_POINT('Ctrl Pts',(3.2819095957713,1.24934477520901,0.699994176777649));
#11304=CARTESIAN_POINT('Ctrl Pts',(3.27712738077041,1.24899781481787,0.699996524298861));
#11305=CARTESIAN_POINT('Ctrl Pts',(3.27235629258357,1.24851338385513,0.699999999330822));
#11306=CARTESIAN_POINT('Ctrl Pts',(3.26760217026193,1.24789200078152,0.699999999999999));
#11307=CARTESIAN_POINT('',(3.15,1.,0.7));
#11308=CARTESIAN_POINT('Origin',(3.3,1.,0.7));
#11309=CARTESIAN_POINT('',(3.15,-1.,0.7));
#11310=CARTESIAN_POINT('Origin',(3.3,-1.,0.7));
#11311=CARTESIAN_POINT('',(1.6,-4.89858719658941E-17,0.7));
#11312=CARTESIAN_POINT('Origin',(2.,0.,0.7));
#11313=CARTESIAN_POINT('Origin',(9.9,-1.,0.8));
#11314=CARTESIAN_POINT('',(9.75,-1.,0.9));
#11315=CARTESIAN_POINT('Origin',(9.9,-1.,0.9));
#11316=CARTESIAN_POINT('',(9.75,-1.,0.7));
#11317=CARTESIAN_POINT('',(9.75,-1.,0.8));
#11318=CARTESIAN_POINT('Origin',(9.9,-1.,0.7));
#11319=CARTESIAN_POINT('Origin',(3.3,-1.,0.8));
#11320=CARTESIAN_POINT('',(3.15,-1.,0.9));
#11321=CARTESIAN_POINT('Origin',(3.3,-1.,0.9));
#11322=CARTESIAN_POINT('',(3.15,-1.,0.8));
#11323=CARTESIAN_POINT('Origin',(3.3,1.,0.8));
#11324=CARTESIAN_POINT('',(3.15,1.,0.9));
#11325=CARTESIAN_POINT('Origin',(3.3,1.,0.9));
#11326=CARTESIAN_POINT('',(3.15,1.,0.8));
#11327=CARTESIAN_POINT('Origin',(9.9,1.,0.8));
#11328=CARTESIAN_POINT('',(9.75,1.,0.9));
#11329=CARTESIAN_POINT('Origin',(9.9,1.,0.9));
#11330=CARTESIAN_POINT('',(9.75,1.,0.7));
#11331=CARTESIAN_POINT('',(9.75,1.,0.8));
#11332=CARTESIAN_POINT('Origin',(9.9,1.,0.7));
#11333=CARTESIAN_POINT('Origin',(11.3732050807569,0.3,0.9));
#11334=CARTESIAN_POINT('',(11.3732050807569,0.3,0.9));
#11335=CARTESIAN_POINT('',(11.5464101615138,0.,0.9));
#11336=CARTESIAN_POINT('',(10.8757685185329,1.16158539931442,0.9));
#11337=CARTESIAN_POINT('',(11.3732050807569,0.3,0.6));
#11338=CARTESIAN_POINT('',(11.3732050807569,0.3,0.9));
#11339=CARTESIAN_POINT('',(11.5464101615138,0.,0.6));
#11340=CARTESIAN_POINT('',(11.5464101615138,0.,0.6));
#11341=CARTESIAN_POINT('',(11.5464101615138,0.,0.9));
#11342=CARTESIAN_POINT('Origin',(11.0267949192431,0.3,0.9));
#11343=CARTESIAN_POINT('',(11.0267949192431,0.3,0.9));
#11344=CARTESIAN_POINT('',(8.95044612996854,0.3,0.9));
#11345=CARTESIAN_POINT('',(11.0267949192431,0.3,0.6));
#11346=CARTESIAN_POINT('',(11.0267949192431,0.3,0.9));
#11347=CARTESIAN_POINT('',(11.3732050807569,0.3,0.6));
#11348=CARTESIAN_POINT('Origin',(10.8535898384862,5.55111512312578E-17,
0.9));
#11349=CARTESIAN_POINT('',(10.8535898384862,4.24230095489963E-17,0.9));
#11350=CARTESIAN_POINT('',(10.3561532762622,-0.86158539931442,0.9));
#11351=CARTESIAN_POINT('',(10.8535898384862,5.55111512312578E-17,0.6));
#11352=CARTESIAN_POINT('',(10.8535898384862,4.24230095489963E-17,0.9));
#11353=CARTESIAN_POINT('',(11.0267949192431,0.3,0.6));
#11354=CARTESIAN_POINT('Origin',(11.0267949192431,-0.3,0.9));
#11355=CARTESIAN_POINT('',(11.0267949192431,-0.3,0.9));
#11356=CARTESIAN_POINT('',(10.4427558166406,0.71158539931442,0.9));
#11357=CARTESIAN_POINT('',(11.0267949192431,-0.3,0.6));
#11358=CARTESIAN_POINT('',(11.0267949192431,-0.3,0.9));
#11359=CARTESIAN_POINT('',(10.8535898384862,4.24230095489963E-17,0.6));
#11360=CARTESIAN_POINT('Origin',(11.3732050807569,-0.3,0.9));
#11361=CARTESIAN_POINT('',(11.3732050807569,-0.3,0.9));
#11362=CARTESIAN_POINT('',(9.12365121072543,-0.3,0.9));
#11363=CARTESIAN_POINT('',(11.3732050807569,-0.3,0.6));
#11364=CARTESIAN_POINT('',(11.3732050807569,-0.3,0.9));
#11365=CARTESIAN_POINT('',(11.0267949192431,-0.3,0.6));
#11366=CARTESIAN_POINT('Origin',(11.5464101615138,0.,0.9));
#11367=CARTESIAN_POINT('',(10.9623710589113,-1.01158539931442,0.9));
#11368=CARTESIAN_POINT('',(11.3732050807569,-0.3,0.6));
#11369=CARTESIAN_POINT('Origin',(11.2,5.55111512312578E-17,0.6));
#11370=CARTESIAN_POINT('',(11.03,-2.0818995585505E-17,0.6));
#11371=CARTESIAN_POINT('Origin',(11.2,0.,0.6));
#11372=CARTESIAN_POINT('Origin',(2.17320508075689,0.3,0.9));
#11373=CARTESIAN_POINT('',(2.17320508075689,0.3,0.9));
#11374=CARTESIAN_POINT('',(2.34641016151378,0.,0.9));
#11375=CARTESIAN_POINT('',(2.82576851853285,-0.830273029389787,0.9));
#11376=CARTESIAN_POINT('',(2.17320508075689,0.3,0.6));
#11377=CARTESIAN_POINT('',(2.17320508075689,0.3,0.9));
#11378=CARTESIAN_POINT('',(2.34641016151378,0.,0.6));
#11379=CARTESIAN_POINT('',(2.34641016151378,0.,0.6));
#11380=CARTESIAN_POINT('',(2.34641016151378,0.,0.9));
#11381=CARTESIAN_POINT('Origin',(1.82679491924311,0.3,0.9));
#11382=CARTESIAN_POINT('',(1.82679491924311,0.3,0.9));
#11383=CARTESIAN_POINT('',(4.35044612996854,0.3,0.9));
#11384=CARTESIAN_POINT('',(1.82679491924311,0.3,0.6));
#11385=CARTESIAN_POINT('',(1.82679491924311,0.3,0.9));
#11386=CARTESIAN_POINT('',(2.17320508075689,0.3,0.6));
#11387=CARTESIAN_POINT('Origin',(1.65358983848622,5.55111512312578E-17,
0.9));
#11388=CARTESIAN_POINT('',(1.65358983848622,4.24230095489963E-17,0.9));
#11389=CARTESIAN_POINT('',(2.30615327626219,1.13027302938979,0.9));
#11390=CARTESIAN_POINT('',(1.65358983848622,5.55111512312578E-17,0.6));
#11391=CARTESIAN_POINT('',(1.65358983848622,4.24230095489963E-17,0.9));
#11392=CARTESIAN_POINT('',(1.82679491924311,0.3,0.6));
#11393=CARTESIAN_POINT('Origin',(1.82679491924311,-0.3,0.9));
#11394=CARTESIAN_POINT('',(1.82679491924311,-0.3,0.9));
#11395=CARTESIAN_POINT('',(2.39275581664063,-1.28027302938979,0.9));
#11396=CARTESIAN_POINT('',(1.82679491924311,-0.3,0.6));
#11397=CARTESIAN_POINT('',(1.82679491924311,-0.3,0.9));
#11398=CARTESIAN_POINT('',(1.65358983848622,4.24230095489963E-17,0.6));
#11399=CARTESIAN_POINT('Origin',(2.17320508075689,-0.3,0.9));
#11400=CARTESIAN_POINT('',(2.17320508075689,-0.3,0.9));
#11401=CARTESIAN_POINT('',(4.52365121072543,-0.3,0.9));
#11402=CARTESIAN_POINT('',(2.17320508075689,-0.3,0.6));
#11403=CARTESIAN_POINT('',(2.17320508075689,-0.3,0.9));
#11404=CARTESIAN_POINT('',(1.82679491924311,-0.3,0.6));
#11405=CARTESIAN_POINT('Origin',(2.34641016151378,0.,0.9));
#11406=CARTESIAN_POINT('',(2.9123710589113,0.980273029389787,0.9));
#11407=CARTESIAN_POINT('',(2.17320508075689,-0.3,0.6));
#11408=CARTESIAN_POINT('Origin',(2.,5.55111512312578E-17,0.6));
#11409=CARTESIAN_POINT('',(1.83,-2.0818995585505E-17,0.6));
#11410=CARTESIAN_POINT('Origin',(2.,0.,0.6));
#11411=CARTESIAN_POINT('Origin',(2.,0.,0.45));
#11412=CARTESIAN_POINT('',(1.83,-2.0818995585505E-17,0.32));
#11413=CARTESIAN_POINT('',(1.83,2.0818995585505E-17,0.45));
#11414=CARTESIAN_POINT('Origin',(2.,0.,0.32));
#11415=CARTESIAN_POINT('Origin',(11.2,0.,0.45));
#11416=CARTESIAN_POINT('',(11.03,-2.0818995585505E-17,0.32));
#11417=CARTESIAN_POINT('',(11.03,2.0818995585505E-17,0.45));
#11418=CARTESIAN_POINT('Origin',(11.2,0.,0.32));
#11419=CARTESIAN_POINT('Origin',(12.4,-0.72,0.32));
#11420=CARTESIAN_POINT('',(0.200274469199584,-0.72,0.));
#11421=CARTESIAN_POINT('',(0.217044958570157,-0.72,0.32));
#11422=CARTESIAN_POINT('',(0.225070308370679,-0.72,0.473132796510599));
#11423=CARTESIAN_POINT('',(0.,-0.72,0.));
#11424=CARTESIAN_POINT('',(9.63649764092939,-0.72,0.));
#11425=CARTESIAN_POINT('',(0.0167704893705732,-0.72,0.32));
#11426=CARTESIAN_POINT('',(0.0253444014197637,-0.72,0.483599987759188));
#11427=CARTESIAN_POINT('',(-0.1,-0.72,0.32));
#11428=CARTESIAN_POINT('Origin',(12.4,-0.72,0.32));
#11429=CARTESIAN_POINT('',(0.9,-0.72,0.32));
#11430=CARTESIAN_POINT('',(0.9,-0.72,0.));
#11431=CARTESIAN_POINT('',(0.9,-0.72,0.16));
#11432=CARTESIAN_POINT('',(1.1,-0.72,0.32));
#11433=CARTESIAN_POINT('',(-0.1,-0.72,0.32));
#11434=CARTESIAN_POINT('',(1.1,-0.72,0.));
#11435=CARTESIAN_POINT('',(1.1,-0.72,0.16));
#11436=CARTESIAN_POINT('',(9.63649764092939,-0.72,0.));
#11437=CARTESIAN_POINT('Origin',(12.4,-0.72,0.32));
#11438=CARTESIAN_POINT('',(4.3,-0.72,0.32));
#11439=CARTESIAN_POINT('',(4.3,-0.72,0.));
#11440=CARTESIAN_POINT('',(4.3,-0.72,0.16));
#11441=CARTESIAN_POINT('',(4.5,-0.72,0.32));
#11442=CARTESIAN_POINT('',(-0.1,-0.72,0.32));
#11443=CARTESIAN_POINT('',(4.5,-0.72,0.));
#11444=CARTESIAN_POINT('',(4.5,-0.72,0.16));
#11445=CARTESIAN_POINT('',(9.63649764092939,-0.72,0.));
#11446=CARTESIAN_POINT('Origin',(12.4,-0.72,0.32));
#11447=CARTESIAN_POINT('',(8.7,-0.72,0.32));
#11448=CARTESIAN_POINT('',(8.7,-0.72,0.));
#11449=CARTESIAN_POINT('',(8.7,-0.72,0.16));
#11450=CARTESIAN_POINT('',(8.9,-0.72,0.32));
#11451=CARTESIAN_POINT('',(-0.1,-0.72,0.32));
#11452=CARTESIAN_POINT('',(8.9,-0.72,0.));
#11453=CARTESIAN_POINT('',(8.9,-0.72,0.16));
#11454=CARTESIAN_POINT('',(9.63649764092939,-0.72,0.));
#11455=CARTESIAN_POINT('Origin',(-0.0999999999999996,0.72,0.32));
#11456=CARTESIAN_POINT('',(0.217044958570158,0.72,0.32));
#11457=CARTESIAN_POINT('',(0.200274469199584,0.72,0.));
#11458=CARTESIAN_POINT('',(0.207951231396534,0.72,0.146481348799182));
#11459=CARTESIAN_POINT('',(0.0167704893705736,0.72,0.32));
#11460=CARTESIAN_POINT('',(12.4,0.72,0.32));
#11461=CARTESIAN_POINT('',(0.,0.72,0.));
#11462=CARTESIAN_POINT('',(0.00822532444561912,0.72,0.156948540047771));
#11463=CARTESIAN_POINT('',(3.38649764092939,0.72,0.));
#11464=CARTESIAN_POINT('Origin',(-0.0999999999999996,0.72,0.32));
#11465=CARTESIAN_POINT('',(0.9,0.72,0.));
#11466=CARTESIAN_POINT('',(0.9,0.72,0.32));
#11467=CARTESIAN_POINT('',(0.9,0.72,0.16));
#11468=CARTESIAN_POINT('',(1.1,0.72,0.));
#11469=CARTESIAN_POINT('',(3.38649764092939,0.72,0.));
#11470=CARTESIAN_POINT('',(1.1,0.72,0.32));
#11471=CARTESIAN_POINT('',(1.1,0.72,0.16));
#11472=CARTESIAN_POINT('',(12.4,0.72,0.32));
#11473=CARTESIAN_POINT('Origin',(-0.0999999999999996,0.72,0.32));
#11474=CARTESIAN_POINT('',(4.3,0.72,0.));
#11475=CARTESIAN_POINT('',(4.3,0.72,0.32));
#11476=CARTESIAN_POINT('',(4.3,0.72,0.16));
#11477=CARTESIAN_POINT('',(4.5,0.72,0.));
#11478=CARTESIAN_POINT('',(3.38649764092939,0.72,0.));
#11479=CARTESIAN_POINT('',(4.5,0.72,0.32));
#11480=CARTESIAN_POINT('',(4.5,0.72,0.16));
#11481=CARTESIAN_POINT('',(12.4,0.72,0.32));
#11482=CARTESIAN_POINT('Origin',(6.15,0.,0.32));
#11483=CARTESIAN_POINT('',(1.6,-4.89858719658941E-17,0.32));
#11484=CARTESIAN_POINT('Origin',(2.,0.,0.32));
#11485=CARTESIAN_POINT('Origin',(6.15,0.,0.32));
#11486=CARTESIAN_POINT('',(10.8,-4.89858719658942E-17,0.32));
#11487=CARTESIAN_POINT('Origin',(11.2,0.,0.32));
#11488=CARTESIAN_POINT('Origin',(6.15,0.,0.32));
#11489=CARTESIAN_POINT('',(0.217044958570157,-0.75,0.32));
#11490=CARTESIAN_POINT('',(0.0167704893705736,-0.75,0.32));
#11491=CARTESIAN_POINT('Origin',(6.15,0.,0.32));
#11492=CARTESIAN_POINT('',(0.9,0.696450594095222,0.32));
#11493=CARTESIAN_POINT('',(1.1,-0.696450594095222,0.32));
#11494=CARTESIAN_POINT('Origin',(6.15,0.,0.32));
#11495=CARTESIAN_POINT('',(4.3,0.742407407407408,0.32));
#11496=CARTESIAN_POINT('',(4.5,-0.742407407407408,0.32));
#11497=CARTESIAN_POINT('Origin',(6.15,0.,0.32));
#11498=CARTESIAN_POINT('',(8.7,0.72,0.32));
#11499=CARTESIAN_POINT('',(8.7,0.844259259259259,0.32));
#11500=CARTESIAN_POINT('',(8.9,0.72,0.32));
#11501=CARTESIAN_POINT('',(12.4,0.72,0.32));
#11502=CARTESIAN_POINT('',(8.9,-0.844259259259259,0.32));
#11503=CARTESIAN_POINT('Origin',(-0.0999999999999996,0.72,0.32));
#11504=CARTESIAN_POINT('',(8.7,0.72,0.));
#11505=CARTESIAN_POINT('',(8.7,0.72,0.16));
#11506=CARTESIAN_POINT('',(8.9,0.72,0.));
#11507=CARTESIAN_POINT('',(3.38649764092939,0.72,0.));
#11508=CARTESIAN_POINT('',(8.9,0.72,0.16));
#11509=CARTESIAN_POINT('Origin',(12.4,1.99376954809806,0.));
#11510=CARTESIAN_POINT('',(12.4,1.91212902562343,0.));
#11511=CARTESIAN_POINT('',(12.4,-1.91212902562343,0.));
#11512=CARTESIAN_POINT('',(12.4,1.99376954809806,0.));
#11513=CARTESIAN_POINT('',(12.4,-1.8833055216247,0.604732563714112));
#11514=CARTESIAN_POINT('Ctrl Pts',(12.4,-1.8833055216247,0.604732563714112));
#11515=CARTESIAN_POINT('Ctrl Pts',(12.4,-1.88809880980762,0.504101072758768));
#11516=CARTESIAN_POINT('Ctrl Pts',(12.4,-1.89289370245628,0.403468941627095));
#11517=CARTESIAN_POINT('Ctrl Pts',(12.4,-1.90250151416087,0.201891903194028));
#11518=CARTESIAN_POINT('Ctrl Pts',(12.4,-1.90731451170285,0.100945553925438));
#11519=CARTESIAN_POINT('Ctrl Pts',(12.4,-1.91212902562343,0.));
#11520=CARTESIAN_POINT('',(12.4,-1.78288409287054,0.7));
#11521=CARTESIAN_POINT('Ctrl Pts',(12.4000000030461,-1.78288409409899,0.7));
#11522=CARTESIAN_POINT('Ctrl Pts',(12.4000000066823,-1.79082830277209,0.699999997040196));
#11523=CARTESIAN_POINT('Ctrl Pts',(12.4000021328137,-1.79871128857748,0.699006690321208));
#11524=CARTESIAN_POINT('Ctrl Pts',(12.4000039827682,-1.8063921320806,0.697119229445379));
#11525=CARTESIAN_POINT('Ctrl Pts',(12.4000049365067,-1.81035196808589,0.69614615460905));
#11526=CARTESIAN_POINT('Ctrl Pts',(12.4000058167808,-1.81425808325963,0.694934510320783));
#11527=CARTESIAN_POINT('Ctrl Pts',(12.400006432968,-1.81808986884151,0.693492707237305));
#11528=CARTESIAN_POINT('Ctrl Pts',(12.4000076352846,-1.82556652433459,0.690679432664999));
#11529=CARTESIAN_POINT('Ctrl Pts',(12.4000076271954,-1.83268048852469,0.687023315130674));
#11530=CARTESIAN_POINT('Ctrl Pts',(12.4000063864816,-1.83928589538344,0.682605693351404));
#11531=CARTESIAN_POINT('Ctrl Pts',(12.4000055969106,-1.84348947395919,0.679794387301037));
#11532=CARTESIAN_POINT('Ctrl Pts',(12.400004329084,-1.84748689691167,0.676673627174617));
#11533=CARTESIAN_POINT('Ctrl Pts',(12.4000032503406,-1.8512341074341,0.673255429390325));
#11534=CARTESIAN_POINT('Ctrl Pts',(12.4000023796213,-1.85425870830395,0.670496394655072));
#11535=CARTESIAN_POINT('Ctrl Pts',(12.4000016297172,-1.85710218072175,0.667559826261508));
#11536=CARTESIAN_POINT('Ctrl Pts',(12.4000016274617,-1.859744520612,0.664455546516084));
#11537=CARTESIAN_POINT('Ctrl Pts',(12.4000016230979,-1.86485672743849,0.658449612092435));
#11538=CARTESIAN_POINT('Ctrl Pts',(12.4000041080363,-1.86921906069885,0.651817317967817));
#11539=CARTESIAN_POINT('Ctrl Pts',(12.40000495371,-1.8727702927896,0.64472299566344));
#11540=CARTESIAN_POINT('Ctrl Pts',(12.4000050555652,-1.8731980125259,0.643868536819953));
#11541=CARTESIAN_POINT('Ctrl Pts',(12.4000051394069,-1.87361391018412,0.643007349425002));
#11542=CARTESIAN_POINT('Ctrl Pts',(12.4000052029357,-1.87401783114888,0.642139703315781));
#11543=CARTESIAN_POINT('Ctrl Pts',(12.4000057294153,-1.87736522853405,0.634949295858174));
#11544=CARTESIAN_POINT('Ctrl Pts',(12.4000043880804,-1.87985460663586,0.627401584261416));
#11545=CARTESIAN_POINT('Ctrl Pts',(12.4000025112034,-1.88143175301701,0.619663949188762));
#11546=CARTESIAN_POINT('Ctrl Pts',(12.4000013193515,-1.88243327046239,0.614750406220363));
#11547=CARTESIAN_POINT('Ctrl Pts',(12.4,-1.88306607129604,0.609759643802656));
#11548=CARTESIAN_POINT('Ctrl Pts',(12.4,-1.8833055216247,0.604732563714112));
#11549=CARTESIAN_POINT('',(12.4,1.78288409287164,0.7));
#11550=CARTESIAN_POINT('',(12.4,0.99688477404903,0.7));
#11551=CARTESIAN_POINT('',(12.4,1.8833055216247,0.604732563714112));
#11552=CARTESIAN_POINT('Ctrl Pts',(12.4,1.8833055216247,0.604732563714112));
#11553=CARTESIAN_POINT('Ctrl Pts',(12.4,1.88292893537322,0.612638709665068));
#11554=CARTESIAN_POINT('Ctrl Pts',(12.4000029905988,1.88158186833012,0.620459457162159));
#11555=CARTESIAN_POINT('Ctrl Pts',(12.400004351969,1.87934739482834,0.62803467841275));
#11556=CARTESIAN_POINT('Ctrl Pts',(12.4000050124983,1.87826324073514,0.631710133556493));
#11557=CARTESIAN_POINT('Ctrl Pts',(12.4000053733669,1.87696936339782,0.63532777623417));
#11558=CARTESIAN_POINT('Ctrl Pts',(12.4000053391329,1.87547104796815,0.638868146717817));
#11559=CARTESIAN_POINT('Ctrl Pts',(12.4000052683671,1.872373843052,0.646186534188034));
#11560=CARTESIAN_POINT('Ctrl Pts',(12.4000032465668,1.86844110215533,0.653093304890266));
#11561=CARTESIAN_POINT('Ctrl Pts',(12.4000021327941,1.86374151467895,0.659427433016556));
#11562=CARTESIAN_POINT('Ctrl Pts',(12.4000018304335,1.86246569800928,0.66114698527342));
#11563=CARTESIAN_POINT('Ctrl Pts',(12.4000016226794,1.86113309763036,0.662824214875179));
#11564=CARTESIAN_POINT('Ctrl Pts',(12.400001625255,1.85974452038344,0.664455546516227));
#11565=CARTESIAN_POINT('Ctrl Pts',(12.4000016287814,1.85784336180007,0.666689070188443));
#11566=CARTESIAN_POINT('Ctrl Pts',(12.400002024929,1.85583728779192,0.668836587948716));
#11567=CARTESIAN_POINT('Ctrl Pts',(12.4000025639666,1.85373364862045,0.670894373083513));
#11568=CARTESIAN_POINT('Ctrl Pts',(12.400004021536,1.84804536272624,0.676458668669153));
#11569=CARTESIAN_POINT('Ctrl Pts',(12.4000062945443,1.84171268252251,0.681305055194542));
#11570=CARTESIAN_POINT('Ctrl Pts',(12.4000070319583,1.83490078417639,0.685381489016216));
#11571=CARTESIAN_POINT('Ctrl Pts',(12.4000075068619,1.8305138392177,0.688006761722114));
#11572=CARTESIAN_POINT('Ctrl Pts',(12.4000074483741,1.82592714021755,0.69031203082117));
#11573=CARTESIAN_POINT('Ctrl Pts',(12.4000068708525,1.82117863971551,0.692273867243687));
#11574=CARTESIAN_POINT('Ctrl Pts',(12.4000059767178,1.81382688138917,0.695311236040001));
#11575=CARTESIAN_POINT('Ctrl Pts',(12.4000038254996,1.80617119073902,0.697493343451155));
#11576=CARTESIAN_POINT('Ctrl Pts',(12.4000020685374,1.7983596509798,0.698751345219246));
#11577=CARTESIAN_POINT('Ctrl Pts',(12.4000009204513,1.79325520389048,0.699573385900268));
#11578=CARTESIAN_POINT('Ctrl Pts',(12.400000005426,1.78808359082883,0.699999998062804));
#11579=CARTESIAN_POINT('Ctrl Pts',(12.4000000030461,1.78288409409899,0.7));
#11580=CARTESIAN_POINT('Ctrl Pts',(12.4,1.91212902562343,0.));
#11581=CARTESIAN_POINT('Ctrl Pts',(12.4,1.90731404243129,0.1009553931071));
#11582=CARTESIAN_POINT('Ctrl Pts',(12.4,1.9025005759122,0.201911581737034));
#11583=CARTESIAN_POINT('Ctrl Pts',(12.4,1.89289276481806,0.403488620176902));
#11584=CARTESIAN_POINT('Ctrl Pts',(12.4,1.88809834114759,0.504110911924693));
#11585=CARTESIAN_POINT('Ctrl Pts',(12.4,1.8833055216247,0.604732563714112));
#11586=CARTESIAN_POINT('Origin',(8.9,-1.68851851851852,0.));
#11587=CARTESIAN_POINT('',(8.9,1.62420669932031,0.));
#11588=CARTESIAN_POINT('',(8.9,-1.68851851851852,0.));
#11589=CARTESIAN_POINT('',(8.9,1.59320117118329,0.605106081470792));
#11590=CARTESIAN_POINT('Ctrl Pts',(8.9,1.59320117118329,0.605106081470792));
#11591=CARTESIAN_POINT('Ctrl Pts',(8.9,1.59837103562161,0.504197738990529));
#11592=CARTESIAN_POINT('Ctrl Pts',(8.9,1.60354126123154,0.403288838380538));
#11593=CARTESIAN_POINT('Ctrl Pts',(8.9,1.61387642009944,0.201587196710533));
#11594=CARTESIAN_POINT('Ctrl Pts',(8.9,1.61904141157348,0.100793304842659));
#11595=CARTESIAN_POINT('Ctrl Pts',(8.9,1.62420669932031,0.));
#11596=CARTESIAN_POINT('',(8.9,1.49312521822106,0.7));
#11597=CARTESIAN_POINT('Ctrl Pts',(8.9,1.49312521822106,0.7));
#11598=CARTESIAN_POINT('Ctrl Pts',(8.9,1.50104136823484,0.7));
#11599=CARTESIAN_POINT('Ctrl Pts',(8.90000131173634,1.50889623314995,0.699007530025307));
#11600=CARTESIAN_POINT('Ctrl Pts',(8.90000245364087,1.51654949575132,0.697121675771258));
#11601=CARTESIAN_POINT('Ctrl Pts',(8.9000030153269,1.52031402289636,0.696194051841344));
#11602=CARTESIAN_POINT('Ctrl Pts',(8.90000353645954,1.52402976767023,0.695049421358208));
#11603=CARTESIAN_POINT('Ctrl Pts',(8.90000391188735,1.52767894577544,0.693695149285802));
#11604=CARTESIAN_POINT('Ctrl Pts',(8.90000468147812,1.53515940869299,0.690919022244083));
#11605=CARTESIAN_POINT('Ctrl Pts',(8.90000470661952,1.54227958804117,0.687295426711095));
#11606=CARTESIAN_POINT('Ctrl Pts',(8.9000039635008,1.54889410374269,0.682907715777054));
#11607=CARTESIAN_POINT('Ctrl Pts',(8.90000349228854,1.55308837416723,0.680125464281631));
#11608=CARTESIAN_POINT('Ctrl Pts',(8.90000272405863,1.55707914411963,0.677034908766328));
#11609=CARTESIAN_POINT('Ctrl Pts',(8.90000205379677,1.56082314136721,0.673648333128258));
#11610=CARTESIAN_POINT('Ctrl Pts',(8.90000149471997,1.56394607304962,0.670823532879853));
#11611=CARTESIAN_POINT('Ctrl Pts',(8.90000100172653,1.56687805273397,0.667809941545923));
#11612=CARTESIAN_POINT('Ctrl Pts',(8.90000100003,1.56959740049228,0.664618488856983));
#11613=CARTESIAN_POINT('Ctrl Pts',(8.90000099684156,1.57470809805256,0.658620525035968));
#11614=CARTESIAN_POINT('Ctrl Pts',(8.90000253934467,1.57907071782202,0.651995745956818));
#11615=CARTESIAN_POINT('Ctrl Pts',(8.90000305932469,1.58262507990443,0.644909256877938));
#11616=CARTESIAN_POINT('Ctrl Pts',(8.90000311559331,1.58300970826793,0.644142406277414));
#11617=CARTESIAN_POINT('Ctrl Pts',(8.9000031627798,1.58338482682255,0.643370127200485));
#11618=CARTESIAN_POINT('Ctrl Pts',(8.90000319981124,1.58375032531468,0.642592615892991));
#11619=CARTESIAN_POINT('Ctrl Pts',(8.90000354178946,1.58712563340961,0.635412448897651));
#11620=CARTESIAN_POINT('Ctrl Pts',(8.90000272882427,1.58964525157545,0.627871187463612));
#11621=CARTESIAN_POINT('Ctrl Pts',(8.90000156924769,1.59125549206429,0.620136848214628));
#11622=CARTESIAN_POINT('Ctrl Pts',(8.90000082792478,1.59228492658837,0.615192247765769));
#11623=CARTESIAN_POINT('Ctrl Pts',(8.89999999997262,1.59294182914154,0.610168076493048));
#11624=CARTESIAN_POINT('Ctrl Pts',(8.9000000009702,1.5932011715731,0.605106081469384));
#11625=CARTESIAN_POINT('',(8.9,-1.49312521822001,0.7));
#11626=CARTESIAN_POINT('',(8.9,-0.844259259259259,0.7));
#11627=CARTESIAN_POINT('',(8.9,-1.59320117118329,0.605106081470792));
#11628=CARTESIAN_POINT('Ctrl Pts',(8.90000000097019,-1.5932011715731,0.605106081469384));
#11629=CARTESIAN_POINT('Ctrl Pts',(8.89999999941083,-1.59279578158415,0.613018716877257));
#11630=CARTESIAN_POINT('Ctrl Pts',(8.90000185372291,-1.59142151714118,0.620841302874248));
#11631=CARTESIAN_POINT('Ctrl Pts',(8.90000269095591,-1.58916270068609,0.628413601005994));
#11632=CARTESIAN_POINT('Ctrl Pts',(8.90000316003867,-1.58789713677684,0.632656188846207));
#11633=CARTESIAN_POINT('Ctrl Pts',(8.90000337414869,-1.58635289833986,0.636820251299613));
#11634=CARTESIAN_POINT('Ctrl Pts',(8.90000326408749,-1.58453800492682,0.640875626603871));
#11635=CARTESIAN_POINT('Ctrl Pts',(8.9000030675631,-1.58129734600662,0.648116871770122));
#11636=CARTESIAN_POINT('Ctrl Pts',(8.90000169351568,-1.5772322800227,0.654932667693845));
#11637=CARTESIAN_POINT('Ctrl Pts',(8.90000116172667,-1.57240747726376,0.66116027211862));
#11638=CARTESIAN_POINT('Ctrl Pts',(8.90000106146602,-1.57149783490479,0.662334391157823));
#11639=CARTESIAN_POINT('Ctrl Pts',(8.90000099955281,-1.57056105641498,0.663487533005214));
#11640=CARTESIAN_POINT('Ctrl Pts',(8.90000100072893,-1.56959740053727,0.664618488856962));
#11641=CARTESIAN_POINT('Ctrl Pts',(8.9000010030487,-1.56769671285427,0.666849154291726));
#11642=CARTESIAN_POINT('Ctrl Pts',(8.90000124864079,-1.56569149899762,0.668993559652069));
#11643=CARTESIAN_POINT('Ctrl Pts',(8.90000158179872,-1.56358911460694,0.671047966011734));
#11644=CARTESIAN_POINT('Ctrl Pts',(8.90000248280001,-1.55790336961918,0.676603957919834));
#11645=CARTESIAN_POINT('Ctrl Pts',(8.90000387848177,-1.55157399841983,0.681441805123218));
#11646=CARTESIAN_POINT('Ctrl Pts',(8.90000432886686,-1.54476515293017,0.68550782533293));
#11647=CARTESIAN_POINT('Ctrl Pts',(8.9000046162921,-1.54041990676133,0.688102664467623));
#11648=CARTESIAN_POINT('Ctrl Pts',(8.90000458123012,-1.53587841548674,0.69038248607508));
#11649=CARTESIAN_POINT('Ctrl Pts',(8.90000422571091,-1.53117752164703,0.692323975790708));
#11650=CARTESIAN_POINT('Ctrl Pts',(8.90000367147839,-1.52384911813356,0.695350638493274));
#11651=CARTESIAN_POINT('Ctrl Pts',(8.9000023358238,-1.51621796414731,0.697522741667433));
#11652=CARTESIAN_POINT('Ctrl Pts',(8.90000125519218,-1.50843132129101,0.698770821080692));
#11653=CARTESIAN_POINT('Ctrl Pts',(8.90000055451733,-1.5033825102871,0.699580068042664));
#11654=CARTESIAN_POINT('Ctrl Pts',(8.9,-1.49826772866746,0.7));
#11655=CARTESIAN_POINT('Ctrl Pts',(8.9,-1.49312521822106,0.7));
#11656=CARTESIAN_POINT('',(8.9,-1.62420669932031,0.));
#11657=CARTESIAN_POINT('Ctrl Pts',(8.9,-1.62420669932031,0.));
#11658=CARTESIAN_POINT('Ctrl Pts',(8.9,-1.61904139377919,0.100793652073202));
#11659=CARTESIAN_POINT('Ctrl Pts',(8.9,-1.61387638451174,0.201587891198165));
#11660=CARTESIAN_POINT('Ctrl Pts',(8.9,-1.60354122564866,0.403289532862703));
#11661=CARTESIAN_POINT('Ctrl Pts',(8.9,-1.59837101783099,0.50419808623799));
#11662=CARTESIAN_POINT('Ctrl Pts',(8.9,-1.59320117118329,0.605106081470792));
#11663=CARTESIAN_POINT('',(8.9,-1.68851851851852,0.));
#11664=CARTESIAN_POINT('Origin',(4.5,-1.48481481481482,0.));
#11665=CARTESIAN_POINT('',(4.5,1.41772989878425,0.));
#11666=CARTESIAN_POINT('',(4.5,-1.48481481481482,0.));
#11667=CARTESIAN_POINT('',(4.5,1.38566996325095,0.605286533624017));
#11668=CARTESIAN_POINT('Ctrl Pts',(4.5,1.38566996325095,0.605286533624017));
#11669=CARTESIAN_POINT('Ctrl Pts',(4.5,1.3910232158183,0.504222354021684));
#11670=CARTESIAN_POINT('Ctrl Pts',(4.5,1.39637635187357,0.403158168247774));
#11671=CARTESIAN_POINT('Ctrl Pts',(4.5,1.4070629957395,0.201395990303158));
#11672=CARTESIAN_POINT('Ctrl Pts',(4.5,1.41239650438775,0.100697998177668));
#11673=CARTESIAN_POINT('Ctrl Pts',(4.5,1.41772989878425,0.));
#11674=CARTESIAN_POINT('',(4.5,1.28575421950843,0.7));
#11675=CARTESIAN_POINT('Ctrl Pts',(4.5,1.28575421950843,0.7));
#11676=CARTESIAN_POINT('Ctrl Pts',(4.5,1.29366545802379,0.7));
#11677=CARTESIAN_POINT('Ctrl Pts',(4.50000067540813,1.30151306508378,0.699006020085879));
#11678=CARTESIAN_POINT('Ctrl Pts',(4.50000126278178,1.30915682219698,0.697118891599074));
#11679=CARTESIAN_POINT('Ctrl Pts',(4.50000159346398,1.31346013814185,0.696056467716811));
#11680=CARTESIAN_POINT('Ctrl Pts',(4.50000189442328,1.31769890045703,0.694709922559592));
#11681=CARTESIAN_POINT('Ctrl Pts',(4.50000208642664,1.32184639782974,0.693090275295953));
#11682=CARTESIAN_POINT('Ctrl Pts',(4.50000243009859,1.32927011415192,0.690191225399894));
#11683=CARTESIAN_POINT('Ctrl Pts',(4.50000235826664,1.33632110693134,0.686451804482762));
#11684=CARTESIAN_POINT('Ctrl Pts',(4.50000192249634,1.34285330390028,0.681953677325188));
#11685=CARTESIAN_POINT('Ctrl Pts',(4.5000016824508,1.3464515866709,0.679475868782656));
#11686=CARTESIAN_POINT('Ctrl Pts',(4.50000134086274,1.34989218134371,0.676766953538005));
#11687=CARTESIAN_POINT('Ctrl Pts',(4.50000103767597,1.35314674504257,0.67383503027087));
#11688=CARTESIAN_POINT('Ctrl Pts',(4.50000074242034,1.35631617169348,0.670979804009792));
#11689=CARTESIAN_POINT('Ctrl Pts',(4.50000047986374,1.35928994516467,0.667930335702103));
#11690=CARTESIAN_POINT('Ctrl Pts',(4.5000004798165,1.36204555935344,0.66469809744354));
#11691=CARTESIAN_POINT('Ctrl Pts',(4.5000004797289,1.36715559606013,0.658704204607119));
#11692=CARTESIAN_POINT('Ctrl Pts',(4.50000128456446,1.3715183542993,0.652083197653858));
#11693=CARTESIAN_POINT('Ctrl Pts',(4.50000155892095,1.37507421485048,0.645000595057188));
#11694=CARTESIAN_POINT('Ctrl Pts',(4.50000158702893,1.37543851484667,0.644274978272754));
#11695=CARTESIAN_POINT('Ctrl Pts',(4.50000161091379,1.37579430519483,0.643544496675346));
#11696=CARTESIAN_POINT('Ctrl Pts',(4.50000163009343,1.37614149316233,0.642809317076966));
#11697=CARTESIAN_POINT('Ctrl Pts',(4.50000181728783,1.37953006709248,0.635633923185928));
#11698=CARTESIAN_POINT('Ctrl Pts',(4.50000140772507,1.38206400387968,0.628095594687559));
#11699=CARTESIAN_POINT('Ctrl Pts',(4.50000081194859,1.38368993781387,0.620362729373495));
#11700=CARTESIAN_POINT('Ctrl Pts',(4.50000042990035,1.38473258588096,0.615403944208116));
#11701=CARTESIAN_POINT('Ctrl Pts',(4.49999999988018,1.38540098970406,0.610364492806037));
#11702=CARTESIAN_POINT('Ctrl Pts',(4.50000000014037,1.38566996330298,0.605286533623957));
#11703=CARTESIAN_POINT('',(4.5,-1.28575421950842,0.7));
#11704=CARTESIAN_POINT('',(4.5,-0.742407407407408,0.7));
#11705=CARTESIAN_POINT('',(4.5,-1.38566996325095,0.605286533624017));
#11706=CARTESIAN_POINT('Ctrl Pts',(4.50000000014037,-1.38566996330298,0.605286533623957));
#11707=CARTESIAN_POINT('Ctrl Pts',(4.49999999973491,-1.38525081272033,0.613199687771457));
#11708=CARTESIAN_POINT('Ctrl Pts',(4.50000095642016,-1.38386419754969,0.62102180968747));
#11709=CARTESIAN_POINT('Ctrl Pts',(4.50000138305812,-1.38159414679432,0.628592503408469));
#11710=CARTESIAN_POINT('Ctrl Pts',(4.50000162118259,-1.38032713666619,0.632818023740444));
#11711=CARTESIAN_POINT('Ctrl Pts',(4.50000172745986,-1.37878391728058,0.636965253716347));
#11712=CARTESIAN_POINT('Ctrl Pts',(4.50000166716583,-1.37697237493585,0.641004309729874));
#11713=CARTESIAN_POINT('Ctrl Pts',(4.50000155916287,-1.37372741146613,0.648239354085419));
#11714=CARTESIAN_POINT('Ctrl Pts',(4.50000084040372,-1.36965973349804,0.655049237033139));
#11715=CARTESIAN_POINT('Ctrl Pts',(4.50000056390271,-1.36483316768901,0.661270759279915));
#11716=CARTESIAN_POINT('Ctrl Pts',(4.50000051219424,-1.36393055121024,0.662434246679675));
#11717=CARTESIAN_POINT('Ctrl Pts',(4.50000048023544,-1.3630012658104,0.663577087492372));
#11718=CARTESIAN_POINT('Ctrl Pts',(4.50000048056391,-1.36204555937839,0.664698097443534));
#11719=CARTESIAN_POINT('Ctrl Pts',(4.50000048121673,-1.36014610273268,0.666926093123284));
#11720=CARTESIAN_POINT('Ctrl Pts',(4.50000060829837,-1.35814231322364,0.669067903674665));
#11721=CARTESIAN_POINT('Ctrl Pts',(4.50000078085101,-1.35604151212276,0.671119765431539));
#11722=CARTESIAN_POINT('Ctrl Pts',(4.50000124774248,-1.3503571825734,0.676671675324794));
#11723=CARTESIAN_POINT('Ctrl Pts',(4.50000197143062,-1.34402953514766,0.681505303070731));
#11724=CARTESIAN_POINT('Ctrl Pts',(4.50000220836427,-1.33722229030693,0.685566265232058));
#11725=CARTESIAN_POINT('Ctrl Pts',(4.50000235894787,-1.33289593407788,0.688147216755564));
#11726=CARTESIAN_POINT('Ctrl Pts',(4.50000234488938,-1.32837489877041,0.690415387400166));
#11727=CARTESIAN_POINT('Ctrl Pts',(4.50000216490635,-1.32369554581057,0.69234752884452));
#11728=CARTESIAN_POINT('Ctrl Pts',(4.50000188343739,-1.31637767466938,0.695369135087455));
#11729=CARTESIAN_POINT('Ctrl Pts',(4.50000119588393,-1.3087575932273,0.697536490026807));
#11730=CARTESIAN_POINT('Ctrl Pts',(4.50000064127173,-1.30098224657147,0.698779892333419));
#11731=CARTESIAN_POINT('Ctrl Pts',(4.50000028296845,-1.29595903898196,0.699583183579437));
#11732=CARTESIAN_POINT('Ctrl Pts',(4.5,-1.29087043558603,0.7));
#11733=CARTESIAN_POINT('Ctrl Pts',(4.5,-1.28575421950843,0.7));
#11734=CARTESIAN_POINT('',(4.5,-1.41772989878425,0.));
#11735=CARTESIAN_POINT('Ctrl Pts',(4.5,-1.41772989878425,0.));
#11736=CARTESIAN_POINT('Ctrl Pts',(4.5,-1.41239649634988,0.100698149937961));
#11737=CARTESIAN_POINT('Ctrl Pts',(4.5,-1.40706297966336,0.201396293824709));
#11738=CARTESIAN_POINT('Ctrl Pts',(4.5,-1.39637633579674,0.403158471769294));
#11739=CARTESIAN_POINT('Ctrl Pts',(4.5,-1.39102320777973,0.504222505781934));
#11740=CARTESIAN_POINT('Ctrl Pts',(4.5,-1.38566996325095,0.605286533624017));
#11741=CARTESIAN_POINT('',(4.5,-1.48481481481482,0.));
#11742=CARTESIAN_POINT('Origin',(1.1,-1.39290118819044,0.));
#11743=CARTESIAN_POINT('',(1.1,1.324891758307,0.));
#11744=CARTESIAN_POINT('',(1.1,-1.39290118819044,0.));
#11745=CARTESIAN_POINT('',(1.10000000295569,1.29254692766489,0.605334652628491));
#11746=CARTESIAN_POINT('Ctrl Pts',(1.10000000295569,1.29254692766489,0.605334652628491));
#11747=CARTESIAN_POINT('Ctrl Pts',(1.10000000295569,1.29794978210809,0.504228164786351));
#11748=CARTESIAN_POINT('Ctrl Pts',(1.1,1.30335245345465,0.403121008362245));
#11749=CARTESIAN_POINT('Ctrl Pts',(1.1,1.31413403739463,0.20134322693425));
#11750=CARTESIAN_POINT('Ctrl Pts',(1.1,1.31951302132877,0.100671299071668));
#11751=CARTESIAN_POINT('Ctrl Pts',(1.1,1.324891758307,0.));
#11752=CARTESIAN_POINT('Ctrl Pts',(1.1,1.19266190204553,0.7));
#11753=CARTESIAN_POINT('Ctrl Pts',(1.1,1.20057109129252,0.7));
#11754=CARTESIAN_POINT('Ctrl Pts',(1.10000046829629,1.20841685974333,0.699006220526237));
#11755=CARTESIAN_POINT('Ctrl Pts',(1.10000087277688,1.21605887983377,0.697119382842322));
#11756=CARTESIAN_POINT('Ctrl Pts',(1.10000109992184,1.22035042410288,0.696059787689036));
#11757=CARTESIAN_POINT('Ctrl Pts',(1.10000130563842,1.22457776983048,0.694717521940989));
#11758=CARTESIAN_POINT('Ctrl Pts',(1.10000143498593,1.22871439246446,0.693103507978966));
#11759=CARTESIAN_POINT('Ctrl Pts',(1.10000166711622,1.23613807995602,0.690206957744321));
#11760=CARTESIAN_POINT('Ctrl Pts',(1.10000160692769,1.24318920265812,0.686469797174223));
#11761=CARTESIAN_POINT('Ctrl Pts',(1.10000129432656,1.24972159507123,0.681973692132557));
#11762=CARTESIAN_POINT('Ctrl Pts',(1.10000112259081,1.25331033895651,0.679503636989594));
#11763=CARTESIAN_POINT('Ctrl Pts',(1.10000088087184,1.25674225826706,0.676803638555143));
#11764=CARTESIAN_POINT('Ctrl Pts',(1.10000066684112,1.25998923415267,0.673881729486736));
#11765=CARTESIAN_POINT('Ctrl Pts',(1.100000457217,1.26316935916797,0.671019978599686));
#11766=CARTESIAN_POINT('Ctrl Pts',(1.1000002715704,1.26615273734033,0.667962699881477));
#11767=CARTESIAN_POINT('Ctrl Pts',(1.1000002731257,1.2689166530284,0.664721467295484));
#11768=CARTESIAN_POINT('Ctrl Pts',(1.10000027600127,1.2740268283512,0.658728785663437));
#11769=CARTESIAN_POINT('Ctrl Pts',(1.10000085014601,1.27838972527875,0.652108677049879));
#11770=CARTESIAN_POINT('Ctrl Pts',(1.1000010530947,1.28194599975408,0.64502688444408));
#11771=CARTESIAN_POINT('Ctrl Pts',(1.10000107362034,1.2823056710724,0.644310652415237));
#11772=CARTESIAN_POINT('Ctrl Pts',(1.10000109127028,1.28265705236355,0.643589678557342));
#11773=CARTESIAN_POINT('Ctrl Pts',(1.10000110571348,1.28300005475086,0.642864123553892));
#11774=CARTESIAN_POINT('Ctrl Pts',(1.10000124853573,1.28639184812822,0.635689442715943));
#11775=CARTESIAN_POINT('Ctrl Pts',(1.10000097361067,1.28892914698194,0.628151301589031));
#11776=CARTESIAN_POINT('Ctrl Pts',(1.10000056283738,1.29055881622654,0.620418355899457));
#11777=CARTESIAN_POINT('Ctrl Pts',(1.10000029930222,1.29160434466024,0.615457217544876));
#11778=CARTESIAN_POINT('Ctrl Pts',(1.0999999999818,1.29227543558766,0.610415225971447));
#11779=CARTESIAN_POINT('Ctrl Pts',(1.1000000000255,1.29254692753179,0.605334652628598));
#11780=CARTESIAN_POINT('',(1.10000000295569,-1.29254692766489,0.605334652628491));
#11781=CARTESIAN_POINT('Ctrl Pts',(1.1000000000255,-1.29254692753179,0.605334652628598));
#11782=CARTESIAN_POINT('Ctrl Pts',(1.09999999995744,-1.29212405100831,0.613248166229861));
#11783=CARTESIAN_POINT('Ctrl Pts',(1.10000066442022,-1.29073420569755,0.621070584654331));
#11784=CARTESIAN_POINT('Ctrl Pts',(1.10000095378343,-1.28846118610397,0.628641296001913));
#11785=CARTESIAN_POINT('Ctrl Pts',(1.10000111506646,-1.28719426797524,0.632861000698125));
#11786=CARTESIAN_POINT('Ctrl Pts',(1.10000118318417,-1.28565198202118,0.637002542581089));
#11787=CARTESIAN_POINT('Ctrl Pts',(1.10000113489265,-1.28384214455607,0.641036116698538));
#11788=CARTESIAN_POINT('Ctrl Pts',(1.10000104828677,-1.28059638744501,0.648269916488365));
#11789=CARTESIAN_POINT('Ctrl Pts',(1.10000053334783,-1.27652829029495,0.655078571385522));
#11790=CARTESIAN_POINT('Ctrl Pts',(1.10000033433257,-1.27170133822839,0.661298646557671));
#11791=CARTESIAN_POINT('Ctrl Pts',(1.10000029715544,-1.27079963749419,0.662460590217389));
#11792=CARTESIAN_POINT('Ctrl Pts',(1.10000027400485,-1.26987132743055,0.663601924550879));
#11793=CARTESIAN_POINT('Ctrl Pts',(1.10000027368829,-1.26891665304159,0.664721467295481));
#11794=CARTESIAN_POINT('Ctrl Pts',(1.10000027305905,-1.2670190620795,0.666946764442229));
#11795=CARTESIAN_POINT('Ctrl Pts',(1.10000036187052,-1.26501734165944,0.669086014589825));
#11796=CARTESIAN_POINT('Ctrl Pts',(1.10000048327469,-1.26291879257262,0.671135465892351));
#11797=CARTESIAN_POINT('Ctrl Pts',(1.10000081209565,-1.25723491092676,0.676686367091516));
#11798=CARTESIAN_POINT('Ctrl Pts',(1.10000132622062,-1.25090760500066,0.68151881845922));
#11799=CARTESIAN_POINT('Ctrl Pts',(1.10000150097561,-1.24410063152763,0.68557843671136));
#11800=CARTESIAN_POINT('Ctrl Pts',(1.10000161196703,-1.2397773464179,0.688156805381407));
#11801=CARTESIAN_POINT('Ctrl Pts',(1.1000016084534,-1.23525961544019,0.690422742497405));
#11802=CARTESIAN_POINT('Ctrl Pts',(1.10000148831111,-1.23058375131837,0.692353039195786));
#11803=CARTESIAN_POINT('Ctrl Pts',(1.10000130031927,-1.22326722442338,0.695373457954986));
#11804=CARTESIAN_POINT('Ctrl Pts',(1.1000008264887,-1.21564857658641,0.697539632783775));
#11805=CARTESIAN_POINT('Ctrl Pts',(1.10000044322439,-1.20787483729518,0.698781928831272));
#11806=CARTESIAN_POINT('Ctrl Pts',(1.1000001958084,-1.20285650563037,0.6995838921283));
#11807=CARTESIAN_POINT('Ctrl Pts',(1.1,-1.19777295102175,0.7));
#11808=CARTESIAN_POINT('Ctrl Pts',(1.1,-1.19266190204553,0.7));
#11809=CARTESIAN_POINT('',(1.1,-1.324891758307,0.));
#11810=CARTESIAN_POINT('Ctrl Pts',(1.1,-1.324891758307,0.));
#11811=CARTESIAN_POINT('Ctrl Pts',(1.1,-1.3195129727271,0.10067220872632));
#11812=CARTESIAN_POINT('Ctrl Pts',(1.1,-1.31413394019217,0.201345046154956));
#11813=CARTESIAN_POINT('Ctrl Pts',(1.1,-1.30335235623932,0.40312282767794));
#11814=CARTESIAN_POINT('Ctrl Pts',(1.10000000295569,-1.29794973349953,0.504229074424201));
#11815=CARTESIAN_POINT('Ctrl Pts',(1.10000000295569,-1.29254692766489,0.605334652628491));
#11816=CARTESIAN_POINT('',(1.1,-1.39290118819044,0.));
#11817=CARTESIAN_POINT('Origin',(0.199725906950915,-1.5,-0.0104671912485888));
#11818=CARTESIAN_POINT('',(0.200274469199584,1.20659878095028,0.));
#11819=CARTESIAN_POINT('',(0.200274469199585,-0.75,0.));
#11820=CARTESIAN_POINT('',(0.231993417893744,1.17491202960101,0.605233595624295));
#11821=CARTESIAN_POINT('Ctrl Pts',(0.200274469199584,1.20659878095028,-9.43255890062389E-18));
#11822=CARTESIAN_POINT('Ctrl Pts',(0.210847451958254,1.19603647956141,0.20174452921517));
#11823=CARTESIAN_POINT('Ctrl Pts',(0.221420434855641,1.18547422886796,0.403489061077219));
#11824=CARTESIAN_POINT('Ctrl Pts',(0.231993417893744,1.17491202960101,0.605233595624295));
#11825=CARTESIAN_POINT('',(0.231993417893744,-1.17491202960101,0.605233595624295));
#11826=CARTESIAN_POINT('',(0.231993417893744,-0.75,0.605233595624295));
#11827=CARTESIAN_POINT('',(0.200274469199584,-1.20659878095028,1.38777878078145E-17));
#11828=CARTESIAN_POINT('Ctrl Pts',(0.231993417893744,-1.17491202960101,
0.605233595624295));
#11829=CARTESIAN_POINT('Ctrl Pts',(0.221420434855641,-1.18547422886796,
0.40348906107722));
#11830=CARTESIAN_POINT('Ctrl Pts',(0.210847451958254,-1.19603647956141,
0.20174452921517));
#11831=CARTESIAN_POINT('Ctrl Pts',(0.200274469199584,-1.20659878095028,
2.0491421059976E-17));
#11832=CARTESIAN_POINT('',(0.200274469199585,-0.75,0.));
#11833=CARTESIAN_POINT('Origin',(6.87299528185878,-3.57834294608796E-18,
0.));
#11834=CARTESIAN_POINT('Ctrl Pts',(8.90000000000001,-1.62420669932031,-3.75133951679985E-17));
#11835=CARTESIAN_POINT('Ctrl Pts',(10.0682843079684,-1.69891080436391,-1.31961514553165E-7));
#11836=CARTESIAN_POINT('Ctrl Pts',(11.2345361392062,-1.79243531443695,-6.44452192334729E-8));
#11837=CARTESIAN_POINT('Ctrl Pts',(12.4000000002382,-1.91212902541327,2.95121624705651E-11));
#11838=CARTESIAN_POINT('Ctrl Pts',(12.4000000002382,1.91212902541327,2.95118849063386E-11));
#11839=CARTESIAN_POINT('Ctrl Pts',(11.2345361911441,1.79243531977099,-6.4445136166539E-8));
#11840=CARTESIAN_POINT('Ctrl Pts',(10.0682843567552,1.69891080748336,-1.31958638870612E-7));
#11841=CARTESIAN_POINT('Ctrl Pts',(8.9,1.62420669932031,6.39679281766448E-17));
#11842=CARTESIAN_POINT('',(8.7,1.61160179736194,0.));
#11843=CARTESIAN_POINT('',(8.7,1.68851851851852,0.));
#11844=CARTESIAN_POINT('Ctrl Pts',(8.70000000002062,1.61160179731554,-3.21507306454832E-13));
#11845=CARTESIAN_POINT('Ctrl Pts',(7.99734938728961,1.56795839277283,5.29471456843263E-9));
#11846=CARTESIAN_POINT('Ctrl Pts',(7.29393815910572,1.53097060499506,-6.44604909847991E-9));
#11847=CARTESIAN_POINT('Ctrl Pts',(6.58949465297818,1.49904250536939,-7.60372244394637E-9));
#11848=CARTESIAN_POINT('Ctrl Pts',(5.94302350041144,1.46974193664425,-8.66612477447903E-9));
#11849=CARTESIAN_POINT('Ctrl Pts',(5.29757001768168,1.44478244743454,1.79883147367388E-8));
#11850=CARTESIAN_POINT('Ctrl Pts',(4.65216233480351,1.42284617839366,3.84107779578714E-9));
#11851=CARTESIAN_POINT('Ctrl Pts',(4.60144142975536,1.4211222642714,2.72928337404163E-9));
#11852=CARTESIAN_POINT('Ctrl Pts',(4.55072080855761,1.41941704699729,1.44770501019496E-9));
#11853=CARTESIAN_POINT('Ctrl Pts',(4.50000000001737,1.41772989873549,-1.00876616052154E-12));
#11854=CARTESIAN_POINT('',(4.3,1.41116952203211,0.));
#11855=CARTESIAN_POINT('',(4.3,1.48481481481482,0.));
#11856=CARTESIAN_POINT('Ctrl Pts',(4.3,1.41116952203211,-1.0790522121662E-15));
#11857=CARTESIAN_POINT('Ctrl Pts',(3.23514221724601,1.37672428690534,3.20725535317031E-8));
#11858=CARTESIAN_POINT('Ctrl Pts',(2.16992716239601,1.34987955958158,4.63097810372671E-9));
#11859=CARTESIAN_POINT('Ctrl Pts',(1.10000000020726,1.32489175811528,-9.82792569252214E-12));
#11860=CARTESIAN_POINT('',(0.9,1.32024227787037,0.));
#11861=CARTESIAN_POINT('',(0.9,1.39290118819044,0.));
#11862=CARTESIAN_POINT('',(0.297857995688647,1.306435779838,0.));
#11863=CARTESIAN_POINT('Ctrl Pts',(0.9,1.32024227787037,-6.93889390390723E-18));
#11864=CARTESIAN_POINT('Ctrl Pts',(0.699470323836888,1.31560060380002,-4.72996299588896E-10));
#11865=CARTESIAN_POINT('Ctrl Pts',(0.498765843889866,1.3110112408976,-1.02277582142263E-13));
#11866=CARTESIAN_POINT('Ctrl Pts',(0.297857995688647,1.306435779838,-1.00157829096748E-16));
#11867=CARTESIAN_POINT('Ctrl Pts',(0.297857995688647,1.306435779838,-1.95156391047391E-17));
#11868=CARTESIAN_POINT('Ctrl Pts',(0.289922476296638,1.30625505685688,-1.46278605970555E-13));
#11869=CARTESIAN_POINT('Ctrl Pts',(0.282050301799808,1.30510306275878,-1.25203502999379E-6));
#11870=CARTESIAN_POINT('Ctrl Pts',(0.274405144964298,1.30305953674341,-1.39678564665046E-6));
#11871=CARTESIAN_POINT('Ctrl Pts',(0.269498922713003,1.30174811919849,-1.48967827287246E-6));
#11872=CARTESIAN_POINT('Ctrl Pts',(0.26468600784495,1.30006837070384,-1.17796618578504E-6));
#11873=CARTESIAN_POINT('Ctrl Pts',(0.260012701218123,1.29803054880949,-5.63923085528507E-7));
#11874=CARTESIAN_POINT('Ctrl Pts',(0.252740988282594,1.29485967708789,3.91534262267771E-7));
#11875=CARTESIAN_POINT('Ctrl Pts',(0.245891302634708,1.2908611961912,2.26944434681222E-6));
#11876=CARTESIAN_POINT('Ctrl Pts',(0.239629152465829,1.28609427281,1.73040332626933E-6));
#11877=CARTESIAN_POINT('Ctrl Pts',(0.238677421334952,1.28536978852616,1.6484790500646E-6));
#11878=CARTESIAN_POINT('Ctrl Pts',(0.23773930716971,1.28462746803483,1.50379952206709E-6));
#11879=CARTESIAN_POINT('Ctrl Pts',(0.236815449960777,1.28386742955246,1.27686598471174E-6));
#11880=CARTESIAN_POINT('Ctrl Pts',(0.233849259515119,1.28142720517261,5.48259784756267E-7));
#11881=CARTESIAN_POINT('Ctrl Pts',(0.231029859162728,1.27880446664625,-1.01231737317126E-6));
#11882=CARTESIAN_POINT('Ctrl Pts',(0.228365947504865,1.27601569667724,-2.73789903475208E-6));
#11883=CARTESIAN_POINT('Ctrl Pts',(0.222875659368053,1.2702680771449,-6.2943009513513E-6));
#11884=CARTESIAN_POINT('Ctrl Pts',(0.218108003769119,1.26388547870891,-1.02458913084139E-5));
#11885=CARTESIAN_POINT('Ctrl Pts',(0.214119068651703,1.25703104885628,-1.16727273233865E-5));
#11886=CARTESIAN_POINT('Ctrl Pts',(0.211608035823831,1.25271618840614,-1.25709199407453E-5));
#11887=CARTESIAN_POINT('Ctrl Pts',(0.209406266788438,1.24821342134138,-1.25531979180244E-5));
#11888=CARTESIAN_POINT('Ctrl Pts',(0.207536767894457,1.24355803714115,-1.16467700682383E-5));
#11889=CARTESIAN_POINT('Ctrl Pts',(0.204585779527196,1.23620955211972,-1.02159812889057E-5));
#11890=CARTESIAN_POINT('Ctrl Pts',(0.20249437279756,1.22856635796309,-6.44823334219156E-6));
#11891=CARTESIAN_POINT('Ctrl Pts',(0.201333199355162,1.22077498745768,-3.37414558979738E-6));
#11892=CARTESIAN_POINT('Ctrl Pts',(0.200635497716839,1.21609347152911,-1.5270519663277E-6));
#11893=CARTESIAN_POINT('Ctrl Pts',(0.200274469246579,1.21135795995708,-3.76748562593766E-12));
#11894=CARTESIAN_POINT('Ctrl Pts',(0.200274469199584,1.20659878095028,6.07153216591882E-18));
#11895=CARTESIAN_POINT('',(-2.81723893694256E-19,1.20714678905882,-2.77862675945125E-17));
#11896=CARTESIAN_POINT('',(0.,-1.5,0.));
#11897=CARTESIAN_POINT('',(0.292751161823634,1.50665779898694,0.));
#11898=CARTESIAN_POINT('Ctrl Pts',(0.292751161823634,1.50665779898694,-4.77048955893622E-17));
#11899=CARTESIAN_POINT('Ctrl Pts',(0.274916014309114,1.50625165707847,3.84528327419955E-12));
#11900=CARTESIAN_POINT('Ctrl Pts',(0.257184594685611,1.50420857033458,-2.03607170333744E-6));
#11901=CARTESIAN_POINT('Ctrl Pts',(0.239764500086274,1.50063675387888,-2.79213621391921E-6));
#11902=CARTESIAN_POINT('Ctrl Pts',(0.222116086584643,1.49701812291205,-3.55811018958082E-6));
#11903=CARTESIAN_POINT('Ctrl Pts',(0.204785660682177,1.49183000356027,-2.9511242418033E-6));
#11904=CARTESIAN_POINT('Ctrl Pts',(0.187998620502071,1.4851341555102,-6.80337370794577E-7));
#11905=CARTESIAN_POINT('Ctrl Pts',(0.185044527596802,1.48395585623842,-2.80736529130144E-7));
#11906=CARTESIAN_POINT('Ctrl Pts',(0.182107319868513,1.48273075079643,1.61255976403501E-7));
#11907=CARTESIAN_POINT('Ctrl Pts',(0.17918831289364,1.48145903083089,6.35063889779883E-7));
#11908=CARTESIAN_POINT('Ctrl Pts',(0.162608037952008,1.47423552404966,3.32634402063389E-6));
#11909=CARTESIAN_POINT('Ctrl Pts',(0.146760254055949,1.46557586252388,7.36741945499403E-6));
#11910=CARTESIAN_POINT('Ctrl Pts',(0.131860714325404,1.4555643673366,8.80872142158042E-6));
#11911=CARTESIAN_POINT('Ctrl Pts',(0.12416804976458,1.45039541073654,9.55286874158632E-6));
#11912=CARTESIAN_POINT('Ctrl Pts',(0.116728404005452,1.44486529627202,9.54902993357918E-6));
#11913=CARTESIAN_POINT('Ctrl Pts',(0.109574210210226,1.43898090192647,7.86258910610491E-6));
#11914=CARTESIAN_POINT('Ctrl Pts',(0.100675189791982,1.43166137062374,5.76484451217541E-6));
#11915=CARTESIAN_POINT('Ctrl Pts',(0.0922175942578585,1.42379373777092,
1.07962821494929E-6));
#11916=CARTESIAN_POINT('Ctrl Pts',(0.0842272493232774,1.41542759110015,
-4.17082519724513E-6));
#11917=CARTESIAN_POINT('Ctrl Pts',(0.0719003514327883,1.40252093480537,
-1.22708263387205E-5));
#11918=CARTESIAN_POINT('Ctrl Pts',(0.0607923942774574,1.38854365509349,
-2.1446290640466E-5));
#11919=CARTESIAN_POINT('Ctrl Pts',(0.0509667079859164,1.37370740939602,
-2.73088451608079E-5));
#11920=CARTESIAN_POINT('Ctrl Pts',(0.040988527714452,1.35864090617899,-3.32623861267576E-5));
#11921=CARTESIAN_POINT('Ctrl Pts',(0.0323319291028794,1.34268723517955,
-3.58272570146011E-5));
#11922=CARTESIAN_POINT('Ctrl Pts',(0.0251054147216294,1.32603775378173,
-3.42048160832586E-5));
#11923=CARTESIAN_POINT('Ctrl Pts',(0.0239557673766072,1.32338903116455,
-3.39467061825833E-5));
#11924=CARTESIAN_POINT('Ctrl Pts',(0.022842414085455,1.32072266145131,-3.35898145907185E-5));
#11925=CARTESIAN_POINT('Ctrl Pts',(0.0217659098422027,1.31803938112476,
-3.31388957009043E-5));
#11926=CARTESIAN_POINT('Ctrl Pts',(0.0146851456525434,1.30038996137917,
-3.01729526055095E-5));
#11927=CARTESIAN_POINT('Ctrl Pts',(0.00925910545076598,1.282173175788,-2.28911926108039E-5));
#11928=CARTESIAN_POINT('Ctrl Pts',(0.0055880418397064,1.26361786690427,
-1.53360241296986E-5));
#11929=CARTESIAN_POINT('Ctrl Pts',(0.00217213684284492,1.24635225152695,
-8.30598038733772E-6));
#11930=CARTESIAN_POINT('Ctrl Pts',(0.000275638047107462,1.2287919996398,
-1.11502351997496E-6));
#11931=CARTESIAN_POINT('Ctrl Pts',(2.78020181985954E-5,1.21111091902543,
-1.13803743790751E-7));
#11932=CARTESIAN_POINT('Ctrl Pts',(9.289355304618E-6,1.20979019141994,-3.90154078055202E-8));
#11933=CARTESIAN_POINT('Ctrl Pts',(3.5054796412911E-11,1.20846879032832,
-2.82152417201308E-12));
#11934=CARTESIAN_POINT('Ctrl Pts',(6.5594231435373E-18,1.20714678905882,
2.42861286636753E-17));
#11935=CARTESIAN_POINT('',(12.8678148030684,2.16300527278356,0.));
#11936=CARTESIAN_POINT('Ctrl Pts',(0.292751161823634,1.50665779898694,0.));
#11937=CARTESIAN_POINT('Ctrl Pts',(4.48443904223854,1.60211086545473,0.));
#11938=CARTESIAN_POINT('Ctrl Pts',(8.67612692265345,1.70561506876628,0.));
#11939=CARTESIAN_POINT('Ctrl Pts',(12.8678148030684,2.16300527278356,0.));
#11940=CARTESIAN_POINT('',(13.2,1.86519007666192,1.29914761427265E-16));
#11941=CARTESIAN_POINT('Ctrl Pts',(13.2,1.86519007666192,1.40512601554121E-16));
#11942=CARTESIAN_POINT('Ctrl Pts',(13.2000000013352,1.88296731840607,9.35191444695304E-11));
#11943=CARTESIAN_POINT('Ctrl Pts',(13.1983511006715,1.90064589040826,-4.81925060583158E-6));
#11944=CARTESIAN_POINT('Ctrl Pts',(13.1951709302004,1.91804121845656,-9.22684518112407E-6));
#11945=CARTESIAN_POINT('Ctrl Pts',(13.1919252271695,1.93579500539423,-1.37252653764835E-5));
#11946=CARTESIAN_POINT('Ctrl Pts',(13.1870840836913,1.95325521073227,-1.77396479500911E-5));
#11947=CARTESIAN_POINT('Ctrl Pts',(13.1807207319279,1.9702167899609,-1.88895599539727E-5));
#11948=CARTESIAN_POINT('Ctrl Pts',(13.179605107926,1.97319049715201,-1.90911627380646E-5));
#11949=CARTESIAN_POINT('Ctrl Pts',(13.1784425783122,1.97614882406338,-1.92137058190342E-5));
#11950=CARTESIAN_POINT('Ctrl Pts',(13.1772333926356,1.97909058504493,-1.92562174744009E-5));
#11951=CARTESIAN_POINT('Ctrl Pts',(13.1703491364924,1.99583891121373,-1.94982490583826E-5));
#11952=CARTESIAN_POINT('Ctrl Pts',(13.1620175712498,2.0119031422279,-1.67925698753361E-5));
#11953=CARTESIAN_POINT('Ctrl Pts',(13.1523342210936,2.02708796667103,-1.30402710852334E-5));
#11954=CARTESIAN_POINT('Ctrl Pts',(13.1443502942575,2.03960786168842,-9.94649893779315E-6));
#11955=CARTESIAN_POINT('Ctrl Pts',(13.1354462980072,2.05153020544825,-6.18593217696112E-6));
#11956=CARTESIAN_POINT('Ctrl Pts',(13.1256528604983,2.06273196126272,-4.73977425690188E-6));
#11957=CARTESIAN_POINT('Ctrl Pts',(13.1217453950533,2.06720132901318,-4.16277439392992E-6));
#11958=CARTESIAN_POINT('Ctrl Pts',(13.1176961215346,2.07155579183536,-3.97575052791371E-6));
#11959=CARTESIAN_POINT('Ctrl Pts',(13.1135113749213,2.07579033931164,-3.99023031318383E-6));
#11960=CARTESIAN_POINT('Ctrl Pts',(13.1009362730034,2.08851509208914,-4.03374185458576E-6));
#11961=CARTESIAN_POINT('Ctrl Pts',(13.0872516297578,2.10004749226926,-5.60236028337187E-6));
#11962=CARTESIAN_POINT('Ctrl Pts',(13.0726646436523,2.11028882659185,-6.03124820804926E-6));
#11963=CARTESIAN_POINT('Ctrl Pts',(13.0580194031224,2.12057106059247,-6.46184893473862E-6));
#11964=CARTESIAN_POINT('Ctrl Pts',(13.0424632957183,2.12955278528135,-5.76500392338198E-6));
#11965=CARTESIAN_POINT('Ctrl Pts',(13.0261754841647,2.13709349482706,-4.98347139369932E-6));
#11966=CARTESIAN_POINT('Ctrl Pts',(13.0233759049672,2.13838960594114,-4.84914013593099E-6));
#11967=CARTESIAN_POINT('Ctrl Pts',(13.0205546633935,2.13964302898522,-4.72077764982159E-6));
#11968=CARTESIAN_POINT('Ctrl Pts',(13.0177126224567,2.14085289970554,-4.61407510358037E-6));
#11969=CARTESIAN_POINT('Ctrl Pts',(13.0148367726024,2.14207716304734,-4.50610322390289E-6));
#11970=CARTESIAN_POINT('Ctrl Pts',(13.0119432782921,2.14325527660784,-4.42172619954107E-6));
#11971=CARTESIAN_POINT('Ctrl Pts',(13.0090331608036,2.14438664763146,-4.38057543634576E-6));
#11972=CARTESIAN_POINT('Ctrl Pts',(12.9922536897216,2.1509100294015,-4.14330390220891E-6));
#11973=CARTESIAN_POINT('Ctrl Pts',(12.9749229882599,2.15588345271621,-5.05640020348117E-6));
#11974=CARTESIAN_POINT('Ctrl Pts',(12.9572550825995,2.15928949382789,-4.85686529648217E-6));
#11975=CARTESIAN_POINT('Ctrl Pts',(12.9529252316797,2.16012420794307,-4.80796553341985E-6));
#11976=CARTESIAN_POINT('Ctrl Pts',(12.9485750628159,2.16086455090717,-4.70814629363608E-6));
#11977=CARTESIAN_POINT('Ctrl Pts',(12.944207640703,2.16150979950679,-4.55317442353944E-6));
#11978=CARTESIAN_POINT('Ctrl Pts',(12.9263774359968,2.16414405704371,-3.92049452767182E-6));
#11979=CARTESIAN_POINT('Ctrl Pts',(12.9083632163621,2.16518216214944,-2.15504024707585E-6));
#11980=CARTESIAN_POINT('Ctrl Pts',(12.8903762705535,2.16459816844574,-9.12104093693782E-7));
#11981=CARTESIAN_POINT('Ctrl Pts',(12.8828459063217,2.16435367528137,-3.91739933400607E-7));
#11982=CARTESIAN_POINT('Ctrl Pts',(12.8753202361859,2.1638242536466,5.87463683432524E-12));
#11983=CARTESIAN_POINT('Ctrl Pts',(12.8678148030684,2.16300527278357,2.8796409701215E-16));
#11984=CARTESIAN_POINT('',(13.2,-1.86519007666192,1.11326398357188E-16));
#11985=CARTESIAN_POINT('',(13.2,2.2,0.));
#11986=CARTESIAN_POINT('',(12.8678148030684,-2.16300527278356,1.38777878078145E-17));
#11987=CARTESIAN_POINT('Ctrl Pts',(12.8678148030684,-2.16300527278357,2.56739074444567E-16));
#11988=CARTESIAN_POINT('Ctrl Pts',(12.8854929372559,-2.16493428409685,8.24591542686399E-11));
#11989=CARTESIAN_POINT('Ctrl Pts',(12.9032520674897,-2.16521372082443,-4.52295339524789E-6));
#11990=CARTESIAN_POINT('Ctrl Pts',(12.9208958607904,-2.1639404182545,-8.68231213275745E-6));
#11991=CARTESIAN_POINT('Ctrl Pts',(12.9389012534027,-2.16264102008682,-1.29269145154966E-5));
#11992=CARTESIAN_POINT('Ctrl Pts',(12.9567880250381,-2.15972433317902,-1.67278855193166E-5));
#11993=CARTESIAN_POINT('Ctrl Pts',(12.9743443410528,-2.15524079327399,-1.78237954457702E-5));
#11994=CARTESIAN_POINT('Ctrl Pts',(12.9774431846623,-2.15444940919484,-1.80172331504298E-5));
#11995=CARTESIAN_POINT('Ctrl Pts',(12.9805316913262,-2.15360908525727,-1.81351031595367E-5));
#11996=CARTESIAN_POINT('Ctrl Pts',(12.9836086301392,-2.15271994254544,-1.81766625580856E-5));
#11997=CARTESIAN_POINT('Ctrl Pts',(13.0010041030966,-2.14769317440371,-1.84116186093898E-5));
#11998=CARTESIAN_POINT('Ctrl Pts',(13.017876958431,-2.14115457229109,-1.5854618169158E-5));
#11999=CARTESIAN_POINT('Ctrl Pts',(13.0340226638693,-2.13317744288338,-1.23136839993165E-5));
#12000=CARTESIAN_POINT('Ctrl Pts',(13.0473215411186,-2.12660684953271,-9.39709115965876E-6));
#12001=CARTESIAN_POINT('Ctrl Pts',(13.060127470267,-2.11905920305061,-5.85016632862467E-6));
#12002=CARTESIAN_POINT('Ctrl Pts',(13.0723151314263,-2.11055132433008,-4.53327195050794E-6));
#12003=CARTESIAN_POINT('Ctrl Pts',(13.0772147086919,-2.10713106111368,-4.00386555564548E-6));
#12004=CARTESIAN_POINT('Ctrl Pts',(13.0820141951123,-2.10355537352593,-3.85636210984559E-6));
#12005=CARTESIAN_POINT('Ctrl Pts',(13.0867078006727,-2.0998301147952,-3.90248451975241E-6));
#12006=CARTESIAN_POINT('Ctrl Pts',(13.1007249787291,-2.08870484782034,-4.04022639510273E-6));
#12007=CARTESIAN_POINT('Ctrl Pts',(13.1136765748478,-2.07634683247102,-5.5945154994439E-6));
#12008=CARTESIAN_POINT('Ctrl Pts',(13.1254414850725,-2.06295113861397,-5.97495381195624E-6));
#12009=CARTESIAN_POINT('Ctrl Pts',(13.1372476314214,-2.04950849272046,-6.35672556443159E-6));
#12010=CARTESIAN_POINT('Ctrl Pts',(13.1478597809499,-2.03501968083851,-5.56609061204695E-6));
#12011=CARTESIAN_POINT('Ctrl Pts',(13.1571184147632,-2.01964723728874,-4.75455255839871E-6));
#12012=CARTESIAN_POINT('Ctrl Pts',(13.158708901902,-2.01700649414547,-4.61514313115074E-6));
#12013=CARTESIAN_POINT('Ctrl Pts',(13.1602593369672,-2.01433961799121,-4.48389992381974E-6));
#12014=CARTESIAN_POINT('Ctrl Pts',(13.1617687665475,-2.01164737048868,-4.37752847101542E-6));
#12015=CARTESIAN_POINT('Ctrl Pts',(13.1632768494098,-2.00895752501823,-4.27125192317111E-6));
#12016=CARTESIAN_POINT('Ctrl Pts',(13.164742106841,-2.00624572954308,-4.19089851494128E-6));
#12017=CARTESIAN_POINT('Ctrl Pts',(13.1661638648313,-2.00351289682408,-4.15637526360595E-6));
#12018=CARTESIAN_POINT('Ctrl Pts',(13.1744716670281,-1.98754405133797,-3.95464448717833E-6));
#12019=CARTESIAN_POINT('Ctrl Pts',(13.181298057795,-1.97085874357403,-5.01850453361653E-6));
#12020=CARTESIAN_POINT('Ctrl Pts',(13.1866022393826,-1.95366776591112,-4.89891140766866E-6));
#12021=CARTESIAN_POINT('Ctrl Pts',(13.1879075264936,-1.94943729958961,-4.86948116225E-6));
#12022=CARTESIAN_POINT('Ctrl Pts',(13.1891204013114,-1.94517611908519,-4.78523710928743E-6));
#12023=CARTESIAN_POINT('Ctrl Pts',(13.1902397948733,-1.94088722910442,-4.64104147683466E-6));
#12024=CARTESIAN_POINT('Ctrl Pts',(13.1947901580114,-1.92345278286841,-4.05488258426869E-6));
#12025=CARTESIAN_POINT('Ctrl Pts',(13.1977733658442,-1.90566244769967,-2.24449026644408E-6));
#12026=CARTESIAN_POINT('Ctrl Pts',(13.1991406030032,-1.88772335428786,-9.50757284845071E-7));
#12027=CARTESIAN_POINT('Ctrl Pts',(13.1997114533543,-1.8802334044254,-4.10596478211383E-7));
#12028=CARTESIAN_POINT('Ctrl Pts',(13.2000000000958,-1.87271737110067,6.9401096738129E-12));
#12029=CARTESIAN_POINT('Ctrl Pts',(13.2,-1.86519007666192,1.81278603239576E-16));
#12030=CARTESIAN_POINT('',(0.292751161823634,-1.50665779898694,-1.38777878078145E-17));
#12031=CARTESIAN_POINT('Ctrl Pts',(12.8678148030684,-2.16300527278356,0.));
#12032=CARTESIAN_POINT('Ctrl Pts',(8.67612692265345,-1.70561506876628,0.));
#12033=CARTESIAN_POINT('Ctrl Pts',(4.48443904223854,-1.60211086545473,0.));
#12034=CARTESIAN_POINT('Ctrl Pts',(0.292751161823634,-1.50665779898694,
0.));
#12035=CARTESIAN_POINT('',(4.02814324098787E-18,-1.20714678905882,5.54818711994559E-17));
#12036=CARTESIAN_POINT('Ctrl Pts',(-2.22044604925031E-16,-1.20714678905882,
-3.98986399474666E-17));
#12037=CARTESIAN_POINT('Ctrl Pts',(2.12382277713531E-10,-1.2249878157372,
-1.35440422383976E-12));
#12038=CARTESIAN_POINT('Ctrl Pts',(0.00163882612763064,-1.24276245549475,
-1.96699749426327E-6));
#12039=CARTESIAN_POINT('Ctrl Pts',(0.00481304415265273,-1.26026068126938,
-2.66007142975038E-6));
#12040=CARTESIAN_POINT('Ctrl Pts',(0.00802873944670128,-1.27798755504872,
-3.36220171040687E-6));
#12041=CARTESIAN_POINT('Ctrl Pts',(0.0128206026099745,-1.29543230475431,
-2.69550948014298E-6));
#12042=CARTESIAN_POINT('Ctrl Pts',(0.0191320595672371,-1.31236817798419,
-4.00401478067381E-7));
#12043=CARTESIAN_POINT('Ctrl Pts',(0.0202443702650641,-1.31535290133701,
4.0809101773195E-9));
#12044=CARTESIAN_POINT('Ctrl Pts',(0.0214039964883031,-1.3183217636574,
4.5005107558061E-7));
#12045=CARTESIAN_POINT('Ctrl Pts',(0.0226107760969305,-1.32127343934773,
9.26779280916758E-7));
#12046=CARTESIAN_POINT('Ctrl Pts',(0.0294548697216842,-1.33801348419941,
3.63048130534217E-6));
#12047=CARTESIAN_POINT('Ctrl Pts',(0.0377511831708778,-1.35405403406083,
7.64722139837078E-6));
#12048=CARTESIAN_POINT('Ctrl Pts',(0.0474204318104353,-1.36917746582299,
9.03443059383348E-6));
#12049=CARTESIAN_POINT('Ctrl Pts',(0.0524109755304394,-1.37698305136733,
9.75040433665629E-6));
#12050=CARTESIAN_POINT('Ctrl Pts',(0.0577680562174045,-1.38454410063597,
9.71159147480002E-6));
#12051=CARTESIAN_POINT('Ctrl Pts',(0.0634855547170043,-1.39182806229354,
7.98761394269614E-6));
#12052=CARTESIAN_POINT('Ctrl Pts',(0.0706048733905122,-1.40089791062835,
5.84095042579577E-6));
#12053=CARTESIAN_POINT('Ctrl Pts',(0.0782829434694699,-1.40953838460506,
1.09773645972912E-6));
#12054=CARTESIAN_POINT('Ctrl Pts',(0.0864706998703675,-1.41772246232928,
-4.21049985396393E-6));
#12055=CARTESIAN_POINT('Ctrl Pts',(0.0990944981487371,-1.43034058886193,
-1.2394683793612E-5));
#12056=CARTESIAN_POINT('Ctrl Pts',(0.112816484288725,-1.44176429483685,
-2.16481703631134E-5));
#12057=CARTESIAN_POINT('Ctrl Pts',(0.127426518150943,-1.45192534842919,
-2.7562374581111E-5));
#12058=CARTESIAN_POINT('Ctrl Pts',(0.142261949549145,-1.46224316253723,
-3.35678206860622E-5));
#12059=CARTESIAN_POINT('Ctrl Pts',(0.158014355623482,-1.47125989363127,
-3.6155642403295E-5));
#12060=CARTESIAN_POINT('Ctrl Pts',(0.17449494651519,-1.47886261331763,-3.45187637154371E-5));
#12061=CARTESIAN_POINT('Ctrl Pts',(0.177115379630184,-1.48007145458801,
-3.42584981007467E-5));
#12062=CARTESIAN_POINT('Ctrl Pts',(0.179754261386328,-1.48124444832217,
-3.38986806574493E-5));
#12063=CARTESIAN_POINT('Ctrl Pts',(0.18241086941249,-1.48238102342202,-3.34441145409493E-5));
#12064=CARTESIAN_POINT('Ctrl Pts',(0.199890279181845,-1.48985922935543,
-3.04532527580594E-5));
#12065=CARTESIAN_POINT('Ctrl Pts',(0.217974246898519,-1.49569663469242,
-2.31073027206853E-5));
#12066=CARTESIAN_POINT('Ctrl Pts',(0.236436446036386,-1.49978781870256,
-1.54828395726751E-5));
#12067=CARTESIAN_POINT('Ctrl Pts',(0.253618559172887,-1.50359533838099,
-8.38702246898572E-6));
#12068=CARTESIAN_POINT('Ctrl Pts',(0.271129804961754,-1.50589051664322,
-1.1237837803371E-6));
#12069=CARTESIAN_POINT('Ctrl Pts',(0.288799387895208,-1.50654014509364,
-1.14426782679271E-7));
#12070=CARTESIAN_POINT('Ctrl Pts',(0.290115790923368,-1.5065885431154,-3.92285953074499E-8));
#12071=CARTESIAN_POINT('Ctrl Pts',(0.291433072638222,-1.50662778343727,
-2.32210426557352E-12));
#12072=CARTESIAN_POINT('Ctrl Pts',(0.292751161823634,-1.50665779898694,
2.86229373536173E-17));
#12073=CARTESIAN_POINT('',(0.,-1.5,0.));
#12074=CARTESIAN_POINT('',(0.297857995688647,-1.306435779838,0.));
#12075=CARTESIAN_POINT('Ctrl Pts',(0.200274469199585,-1.20659878095028,
-5.63785129692462E-18));
#12076=CARTESIAN_POINT('Ctrl Pts',(0.200274469233139,-1.21453676310593,
-8.71436967499621E-13));
#12077=CARTESIAN_POINT('Ctrl Pts',(0.201246859971722,-1.22243356087926,
-1.21395871814677E-6));
#12078=CARTESIAN_POINT('Ctrl Pts',(0.203115675186186,-1.23012372049816,
-1.3343733317444E-6));
#12079=CARTESIAN_POINT('Ctrl Pts',(0.204315340901654,-1.23506033529553,
-1.41167219064517E-6));
#12080=CARTESIAN_POINT('Ctrl Pts',(0.20588557457721,-1.23991201018842,-1.08820351238587E-6));
#12081=CARTESIAN_POINT('Ctrl Pts',(0.207817175189242,-1.24463217458037,
-4.7123943162984E-7));
#12082=CARTESIAN_POINT('Ctrl Pts',(0.210821635148072,-1.25197403646754,
4.8840194822981E-7));
#12083=CARTESIAN_POINT('Ctrl Pts',(0.214662962735955,-1.25891288736431,
2.34840446672759E-6));
#12084=CARTESIAN_POINT('Ctrl Pts',(0.219285851586231,-1.26528190572196,
1.77850405974346E-6));
#12085=CARTESIAN_POINT('Ctrl Pts',(0.219987799701267,-1.26624898941694,
1.69196931287913E-6));
#12086=CARTESIAN_POINT('Ctrl Pts',(0.220707854727247,-1.26720289123473,
1.54254180957111E-6));
#12087=CARTESIAN_POINT('Ctrl Pts',(0.221445913570039,-1.26814297034805,
1.31084431541716E-6));
#12088=CARTESIAN_POINT('Ctrl Pts',(0.223819423285066,-1.27116615329633,
5.65732650279818E-7));
#12089=CARTESIAN_POINT('Ctrl Pts',(0.226378993511503,-1.27404655624932,
-1.0141799309673E-6));
#12090=CARTESIAN_POINT('Ctrl Pts',(0.229108317341547,-1.27677508245113,
-2.75886047820546E-6));
#12091=CARTESIAN_POINT('Ctrl Pts',(0.234729699316268,-1.28239482161129,
-6.35224711555937E-6));
#12092=CARTESIAN_POINT('Ctrl Pts',(0.241002345945823,-1.28730653457646,
-1.03364935932408E-5));
#12093=CARTESIAN_POINT('Ctrl Pts',(0.247764463424355,-1.29145035967733,
-1.17765252099068E-5));
#12094=CARTESIAN_POINT('Ctrl Pts',(0.25202072563572,-1.29405859685204,-1.26829206064147E-5));
#12095=CARTESIAN_POINT('Ctrl Pts',(0.25647185453211,-1.29636195369988,-1.26655904667795E-5));
#12096=CARTESIAN_POINT('Ctrl Pts',(0.261083107941716,-1.29833661269995,
-1.17517412599227E-5));
#12097=CARTESIAN_POINT('Ctrl Pts',(0.268362152520619,-1.30145368947124,
-1.0309194402435E-5));
#12098=CARTESIAN_POINT('Ctrl Pts',(0.275955349537693,-1.30371808689536,
-6.50743389458559E-6));
#12099=CARTESIAN_POINT('Ctrl Pts',(0.283717840216357,-1.30505580179168,
-3.40467605837577E-6));
#12100=CARTESIAN_POINT('Ctrl Pts',(0.288379557365255,-1.3058591584372,-1.54133347766382E-6));
#12101=CARTESIAN_POINT('Ctrl Pts',(0.293102847896135,-1.30632748638856,
-3.09915230996644E-12));
#12102=CARTESIAN_POINT('Ctrl Pts',(0.297857995688647,-1.306435779838,2.90566182226115E-17));
#12103=CARTESIAN_POINT('',(0.9,-1.32024227787037,0.));
#12104=CARTESIAN_POINT('Ctrl Pts',(0.297857995688651,-1.306435779838,-5.81335652359571E-17));
#12105=CARTESIAN_POINT('Ctrl Pts',(0.498765834064439,-1.31101124067384,
-1.02216845336465E-13));
#12106=CARTESIAN_POINT('Ctrl Pts',(0.699470314209512,-1.31560060357718,
-4.73070532165219E-10));
#12107=CARTESIAN_POINT('Ctrl Pts',(0.9,-1.32024227787037,4.62320796019307E-17));
#12108=CARTESIAN_POINT('',(0.9,1.39290118819044,0.));
#12109=CARTESIAN_POINT('',(4.3,-1.41116952203211,0.));
#12110=CARTESIAN_POINT('Ctrl Pts',(1.10000000020724,-1.32489175811528,-9.82782277325449E-12));
#12111=CARTESIAN_POINT('Ctrl Pts',(2.16992692797068,-1.34987955410658,4.63225598025733E-9));
#12112=CARTESIAN_POINT('Ctrl Pts',(3.23514201430925,-1.37672428034078,3.20747301048384E-8));
#12113=CARTESIAN_POINT('Ctrl Pts',(4.3,-1.41116952203211,-8.74629427996717E-16));
#12114=CARTESIAN_POINT('',(4.3,1.48481481481482,0.));
#12115=CARTESIAN_POINT('',(8.7,-1.61160179736194,0.));
#12116=CARTESIAN_POINT('Ctrl Pts',(4.50000000001737,-1.41772989873549,-1.00870158580013E-12));
#12117=CARTESIAN_POINT('Ctrl Pts',(5.14541122039116,-1.43919849219739,1.84287460122322E-8));
#12118=CARTESIAN_POINT('Ctrl Pts',(5.79079200637672,-1.46358894290692,-2.29215846350395E-9));
#12119=CARTESIAN_POINT('Ctrl Pts',(6.43711407552466,-1.49221504703413,-7.12038357450289E-9));
#12120=CARTESIAN_POINT('Ctrl Pts',(6.48784335049204,-1.49446188584227,-7.49934689782436E-9));
#12121=CARTESIAN_POINT('Ctrl Pts',(6.5385784252675,-1.49673484630497,-7.6873350528488E-9));
#12122=CARTESIAN_POINT('Ctrl Pts',(6.58931977021612,-1.49903457911226,-7.60400982311631E-9));
#12123=CARTESIAN_POINT('Ctrl Pts',(7.29382172663923,-1.5309644828944,-6.44710735180711E-9));
#12124=CARTESIAN_POINT('Ctrl Pts',(7.99729122590638,-1.56795478022256,5.29179522587699E-9));
#12125=CARTESIAN_POINT('Ctrl Pts',(8.70000000002062,-1.61160179731554,-3.21479112539667E-13));
#12126=CARTESIAN_POINT('',(8.7,1.68851851851852,0.));
#12127=CARTESIAN_POINT('',(12.6,-1.93292824674167,0.));
#12128=CARTESIAN_POINT('',(12.8889963716306,-1.96391015057091,0.));
#12129=CARTESIAN_POINT('Ctrl Pts',(12.6000000004653,-1.93292824679067,-1.00288700954909E-16));
#12130=CARTESIAN_POINT('Ctrl Pts',(12.6963367945484,-1.94307238002033,2.28133307867826E-10));
#12131=CARTESIAN_POINT('Ctrl Pts',(12.7926686848896,-1.9533982851754,-5.07154825701885E-13));
#12132=CARTESIAN_POINT('Ctrl Pts',(12.8889963716306,-1.96391015057091,2.24786696790336E-16));
#12133=CARTESIAN_POINT('',(12.9997255308004,-1.86463850151065,-1.38777878078145E-17));
#12134=CARTESIAN_POINT('Ctrl Pts',(12.8889963716306,-1.96391015057091,5.29090660172926E-17));
#12135=CARTESIAN_POINT('Ctrl Pts',(12.8968843421745,-1.96477093437063,1.28387508960266E-11));
#12136=CARTESIAN_POINT('Ctrl Pts',(12.9048206871516,-1.96464841285931,-2.5989605143924E-6));
#12137=CARTESIAN_POINT('Ctrl Pts',(12.9126487282508,-1.9636130141884,-4.24292438262167E-6));
#12138=CARTESIAN_POINT('Ctrl Pts',(12.9176900487482,-1.96294620923983,-5.30165014054907E-6));
#12139=CARTESIAN_POINT('Ctrl Pts',(12.9226867577298,-1.96189962975099,-6.00943773338864E-6));
#12140=CARTESIAN_POINT('Ctrl Pts',(12.9275953864907,-1.96048085896027,-6.09358828708331E-6));
#12141=CARTESIAN_POINT('Ctrl Pts',(12.9352257743335,-1.95827540160737,-6.22439902734509E-6));
#12142=CARTESIAN_POINT('Ctrl Pts',(12.9425549137553,-1.95519874430406,-4.64402662178521E-6));
#12143=CARTESIAN_POINT('Ctrl Pts',(12.949425376669,-1.9513005478593,-3.15156624759025E-6));
#12144=CARTESIAN_POINT('Ctrl Pts',(12.9520760960011,-1.94979656991686,-2.57575445499556E-6));
#12145=CARTESIAN_POINT('Ctrl Pts',(12.9546583803074,-1.94816978416017,-2.04880625960079E-6));
#12146=CARTESIAN_POINT('Ctrl Pts',(12.9571622133441,-1.9464211898676,-1.82278374303809E-6));
#12147=CARTESIAN_POINT('Ctrl Pts',(12.9587955877505,-1.9452804951316,-1.67533805140214E-6));
#12148=CARTESIAN_POINT('Ctrl Pts',(12.9603955609302,-1.94408794089591,-1.65796127395168E-6));
#12149=CARTESIAN_POINT('Ctrl Pts',(12.9619602112942,-1.94284549575182,-1.70649031798611E-6));
#12150=CARTESIAN_POINT('Ctrl Pts',(12.9681665721336,-1.93791719798967,-1.89898620422551E-6));
#12151=CARTESIAN_POINT('Ctrl Pts',(12.9737470546445,-1.93226498850035,-2.8025064238469E-6));
#12152=CARTESIAN_POINT('Ctrl Pts',(12.9786034821464,-1.926037248212,-2.79230211737029E-6));
#12153=CARTESIAN_POINT('Ctrl Pts',(12.9817011960737,-1.92206483066456,-2.78579321297956E-6));
#12154=CARTESIAN_POINT('Ctrl Pts',(12.9845038017717,-1.91785723501915,-2.48811564693169E-6));
#12155=CARTESIAN_POINT('Ctrl Pts',(12.9869771252785,-1.91344616543364,-2.2918341012218E-6));
#12156=CARTESIAN_POINT('Ctrl Pts',(12.9874796596041,-1.91254991636901,-2.25195326317628E-6));
#12157=CARTESIAN_POINT('Ctrl Pts',(12.9879679417815,-1.9116463809131,-2.21866365029432E-6));
#12158=CARTESIAN_POINT('Ctrl Pts',(12.98844174868,-1.91073586520696,-2.19841011183313E-6));
#12159=CARTESIAN_POINT('Ctrl Pts',(12.9918929665356,-1.9041036526468,-2.05088297829219E-6));
#12160=CARTESIAN_POINT('Ctrl Pts',(12.9945793344589,-1.89710244289626,-2.35789128083535E-6));
#12161=CARTESIAN_POINT('Ctrl Pts',(12.9964698429198,-1.88986530397042,-1.93853625224654E-6));
#12162=CARTESIAN_POINT('Ctrl Pts',(12.9984668213505,-1.88222058265133,-1.49556391743615E-6));
#12163=CARTESIAN_POINT('Ctrl Pts',(12.9995610814633,-1.87437060764114,-2.4459616079733E-7));
#12164=CARTESIAN_POINT('Ctrl Pts',(12.9997084424383,-1.86646992060833,-2.60951667192209E-8));
#12165=CARTESIAN_POINT('Ctrl Pts',(12.9997198235207,-1.86585972940924,-9.21975031242219E-9));
#12166=CARTESIAN_POINT('Ctrl Pts',(12.9997255308031,-1.86524923282631,2.14479566203628E-13));
#12167=CARTESIAN_POINT('Ctrl Pts',(12.9997255308004,-1.86463850151065,-9.54097911787244E-18));
#12168=CARTESIAN_POINT('',(12.9997255308004,1.86463850151064,1.38777878078145E-17));
#12169=CARTESIAN_POINT('',(12.9997255308004,1.1,0.));
#12170=CARTESIAN_POINT('',(12.8889963716306,1.96391015057091,0.));
#12171=CARTESIAN_POINT('Ctrl Pts',(12.9997255308004,1.86463850151065,-9.97465998686664E-18));
#12172=CARTESIAN_POINT('Ctrl Pts',(12.9997255309996,1.87257112921612,1.42345874390777E-11));
#12173=CARTESIAN_POINT('Ctrl Pts',(12.9987425107347,1.88044501776258,-2.76622459581243E-6));
#12174=CARTESIAN_POINT('Ctrl Pts',(12.9968635501128,1.8881121101061,-4.50602169498049E-6));
#12175=CARTESIAN_POINT('Ctrl Pts',(12.9956551765012,1.89304287446485,-5.62489820561454E-6));
#12176=CARTESIAN_POINT('Ctrl Pts',(12.994075066483,1.89788828888188,-6.37205869803057E-6));
#12177=CARTESIAN_POINT('Ctrl Pts',(12.9921354490207,1.90260616696402,-6.45954116508302E-6));
#12178=CARTESIAN_POINT('Ctrl Pts',(12.9891151690915,1.90995262200289,-6.59576469602218E-6));
#12179=CARTESIAN_POINT('Ctrl Pts',(12.9852608829945,1.91690476599405,-4.92589918404109E-6));
#12180=CARTESIAN_POINT('Ctrl Pts',(12.9806393828366,1.92331154882078,-3.3382766296878E-6));
#12181=CARTESIAN_POINT('Ctrl Pts',(12.9788533632605,1.92578750666072,-2.72472586378502E-6));
#12182=CARTESIAN_POINT('Ctrl Pts',(12.9769522584487,1.92818179997524,-2.1610482659023E-6));
#12183=CARTESIAN_POINT('Ctrl Pts',(12.9749381758772,1.93048453804291,-1.90960564360578E-6));
#12184=CARTESIAN_POINT('Ctrl Pts',(12.9736352090466,1.93197424425657,-1.74694031832382E-6));
#12185=CARTESIAN_POINT('Ctrl Pts',(12.9722849384098,1.93342561524533,-1.71698229815602E-6));
#12186=CARTESIAN_POINT('Ctrl Pts',(12.9708894910408,1.9348369915754,-1.75552529092739E-6));
#12187=CARTESIAN_POINT('Ctrl Pts',(12.9653179015399,1.94047218048862,-1.90941553332435E-6));
#12188=CARTESIAN_POINT('Ctrl Pts',(12.9590944588136,1.94540670303376,-2.83773366290493E-6));
#12189=CARTESIAN_POINT('Ctrl Pts',(12.9523775255978,1.94955941520082,-2.8574013135715E-6));
#12190=CARTESIAN_POINT('Ctrl Pts',(12.9480923984168,1.95220867479748,-2.86994846593266E-6));
#12191=CARTESIAN_POINT('Ctrl Pts',(12.9436054681019,1.95453912223498,-2.59559485065602E-6));
#12192=CARTESIAN_POINT('Ctrl Pts',(12.9389519978263,1.95652032281755,-2.39773084743613E-6));
#12193=CARTESIAN_POINT('Ctrl Pts',(12.9379934875219,1.95692840561619,-2.35697530915642E-6));
#12194=CARTESIAN_POINT('Ctrl Pts',(12.9370291206935,1.95732112306527,-2.32193094846859E-6));
#12195=CARTESIAN_POINT('Ctrl Pts',(12.9360592398442,1.95769827921557,-2.29894501965994E-6));
#12196=CARTESIAN_POINT('Ctrl Pts',(12.929096105975,1.96040602292032,-2.13392052256244E-6));
#12197=CARTESIAN_POINT('Ctrl Pts',(12.9218497638689,1.96231496375013,-2.36509085467933E-6));
#12198=CARTESIAN_POINT('Ctrl Pts',(12.9144555496645,1.96340894166242,-1.92146179377921E-6));
#12199=CARTESIAN_POINT('Ctrl Pts',(12.9066371708262,1.96456567495722,-1.45238421961943E-6));
#12200=CARTESIAN_POINT('Ctrl Pts',(12.8987125532455,1.96480297730229,-2.37321368026999E-7));
#12201=CARTESIAN_POINT('Ctrl Pts',(12.8908401755085,1.96409377829808,-2.55627471131237E-8));
#12202=CARTESIAN_POINT('Ctrl Pts',(12.89022523009,1.96403837970149,-9.02136684357828E-9));
#12203=CARTESIAN_POINT('Ctrl Pts',(12.8896106033158,1.96397717928728,1.9621770460073E-13));
#12204=CARTESIAN_POINT('Ctrl Pts',(12.8889963716306,1.96391015057091,-3.29597460435593E-17));
#12205=CARTESIAN_POINT('',(12.6,1.93292824674167,0.));
#12206=CARTESIAN_POINT('Ctrl Pts',(12.8889963716306,1.96391015057091,8.95144418658345E-17));
#12207=CARTESIAN_POINT('Ctrl Pts',(12.7926686852738,1.95339828521733,-5.07275478770449E-13));
#12208=CARTESIAN_POINT('Ctrl Pts',(12.6963367949308,1.94307238006059,2.28132759158623E-10));
#12209=CARTESIAN_POINT('Ctrl Pts',(12.6000000004652,1.93292824679066,-1.5019386425618E-16));
#12210=CARTESIAN_POINT('',(12.6,-1.99376954809806,0.));
#12211=CARTESIAN_POINT('Origin',(11.2,0.,0.));
#12212=CARTESIAN_POINT('',(10.8,-4.89858719658942E-17,0.7));
#12213=CARTESIAN_POINT('Origin',(11.2,0.,0.7));
#12214=CARTESIAN_POINT('',(10.8,-4.89858719658942E-17,0.));
#12215=CARTESIAN_POINT('Origin',(2.,0.,0.));
#12216=CARTESIAN_POINT('',(1.6,-4.89858719658941E-17,0.));
#12217=CARTESIAN_POINT('Origin',(12.6,-1.99376954809806,0.));
#12218=CARTESIAN_POINT('',(12.6,-1.90428042248893,0.60470250816874));
#12219=CARTESIAN_POINT('Ctrl Pts',(12.6,-1.93292824674167,0.));
#12220=CARTESIAN_POINT('Ctrl Pts',(12.6,-1.92814118331811,0.100975624959503));
#12221=CARTESIAN_POINT('Ctrl Pts',(12.6,-1.9233557423333,0.20195205683881));
#12222=CARTESIAN_POINT('Ctrl Pts',(12.6,-1.91380649287245,0.40351907263528));
#12223=CARTESIAN_POINT('Ctrl Pts',(12.6,-1.90904260275794,0.504111110768618));
#12224=CARTESIAN_POINT('Ctrl Pts',(12.6,-1.90428042248893,0.60470250816874));
#12225=CARTESIAN_POINT('',(12.6,1.90428042248893,0.60470250816874));
#12226=CARTESIAN_POINT('Ctrl Pts',(12.6,1.90428042248893,0.60470250816874));
#12227=CARTESIAN_POINT('Ctrl Pts',(12.6,1.90904310126474,0.504100580823831));
#12228=CARTESIAN_POINT('Ctrl Pts',(12.6,1.91380749024866,0.403498012513773));
#12229=CARTESIAN_POINT('Ctrl Pts',(12.6,1.92335674041114,0.201930996640285));
#12230=CARTESIAN_POINT('Ctrl Pts',(12.6,1.92814168252712,0.100965094925255));
#12231=CARTESIAN_POINT('Ctrl Pts',(12.6,1.93292824674167,0.));
#12232=CARTESIAN_POINT('',(12.6,1.80383022254432,0.7));
#12233=CARTESIAN_POINT('Ctrl Pts',(12.6,1.80383022254432,0.7));
#12234=CARTESIAN_POINT('Ctrl Pts',(12.6,1.81177675668304,0.7));
#12235=CARTESIAN_POINT('Ctrl Pts',(12.6000021803669,1.81966206665253,0.699006623620781));
#12236=CARTESIAN_POINT('Ctrl Pts',(12.6000040789681,1.8273451885609,0.69711902809518));
#12237=CARTESIAN_POINT('Ctrl Pts',(12.6000050614635,1.8313210797205,0.696142227980247));
#12238=CARTESIAN_POINT('Ctrl Pts',(12.6000059683507,1.83524283435206,0.694925046992878));
#12239=CARTESIAN_POINT('Ctrl Pts',(12.6000066021136,1.83908960013903,0.693475985595303));
#12240=CARTESIAN_POINT('Ctrl Pts',(12.6000078338507,1.84656590463324,0.690659691378536));
#12241=CARTESIAN_POINT('Ctrl Pts',(12.6000078244032,1.85367932786264,0.687000939374075));
#12242=CARTESIAN_POINT('Ctrl Pts',(12.6000065509639,1.86028396908448,0.682580904467878));
#12243=CARTESIAN_POINT('Ctrl Pts',(12.600005740321,1.86448833536622,0.679767209507086));
#12244=CARTESIAN_POINT('Ctrl Pts',(12.6000044390918,1.86848632867783,0.676643963831362));
#12245=CARTESIAN_POINT('Ctrl Pts',(12.6000033339006,1.8722338275817,0.673223162566374));
#12246=CARTESIAN_POINT('Ctrl Pts',(12.6000024442799,1.87525036668517,0.670469597843409));
#12247=CARTESIAN_POINT('Ctrl Pts',(12.600001679327,1.8780865799519,0.667539409933064));
#12248=CARTESIAN_POINT('Ctrl Pts',(12.600001676908,1.88072259809992,0.664442334323256));
#12249=CARTESIAN_POINT('Ctrl Pts',(12.6000016722164,1.88583495965423,0.658435786041233));
#12250=CARTESIAN_POINT('Ctrl Pts',(12.6000042182276,1.89019731592974,0.651802923597933));
#12251=CARTESIAN_POINT('Ctrl Pts',(12.6000050838539,1.89374834224248,0.644708005294394));
#12252=CARTESIAN_POINT('Ctrl Pts',(12.60000518898,1.89417959722901,0.643846361750254));
#12253=CARTESIAN_POINT('Ctrl Pts',(12.6000052753339,1.8945988291305,0.642977876839351));
#12254=CARTESIAN_POINT('Ctrl Pts',(12.6000053405091,1.89500587920016,0.642102827114796));
#12255=CARTESIAN_POINT('Ctrl Pts',(12.6000058761205,1.89835102950234,0.634911640898031));
#12256=CARTESIAN_POINT('Ctrl Pts',(12.6000044960414,1.90083797337412,0.627363460372113));
#12257=CARTESIAN_POINT('Ctrl Pts',(12.6000025707297,1.90241244660326,0.619625605651968));
#12258=CARTESIAN_POINT('Ctrl Pts',(12.6000013488022,1.90341170938816,0.614714661398562));
#12259=CARTESIAN_POINT('Ctrl Pts',(12.5999999979477,1.90404256918024,0.609726685483646));
#12260=CARTESIAN_POINT('Ctrl Pts',(12.6000000000242,1.90428042250026,0.604702508168697));
#12261=CARTESIAN_POINT('',(12.6,-1.8038302225439,0.7));
#12262=CARTESIAN_POINT('',(12.6,-0.996884774049031,0.7));
#12263=CARTESIAN_POINT('Ctrl Pts',(12.6000000000242,-1.90428042250026,0.604702508168697));
#12264=CARTESIAN_POINT('Ctrl Pts',(12.5999999967566,-1.90390613686288,0.612608546261599));
#12265=CARTESIAN_POINT('Ctrl Pts',(12.6000030637542,-1.90256112855112,0.620429349781532));
#12266=CARTESIAN_POINT('Ctrl Pts',(12.6000044618611,-1.90032851942705,0.628004813168584));
#12267=CARTESIAN_POINT('Ctrl Pts',(12.6000051410147,-1.89924399238468,0.63168472059761));
#12268=CARTESIAN_POINT('Ctrl Pts',(12.6000055125137,-1.89794920179963,0.635306724151721));
#12269=CARTESIAN_POINT('Ctrl Pts',(12.6000054780251,-1.8964494555225,0.638851301608537));
#12270=CARTESIAN_POINT('Ctrl Pts',(12.6000054068101,-1.89335265044601,0.64617044994032));
#12271=CARTESIAN_POINT('Ctrl Pts',(12.6000033360581,-1.88942004582711,0.653077891556402));
#12272=CARTESIAN_POINT('Ctrl Pts',(12.6000021947065,-1.88472046879005,0.659412676045522));
#12273=CARTESIAN_POINT('Ctrl Pts',(12.6000018847951,-1.88344439178375,0.661132761228218));
#12274=CARTESIAN_POINT('Ctrl Pts',(12.6000016718208,-1.88211149822114,0.662810505670431));
#12275=CARTESIAN_POINT('Ctrl Pts',(12.6000016744967,-1.88072259784382,0.664442334323417));
#12276=CARTESIAN_POINT('Ctrl Pts',(12.6000016781594,-1.87882150924004,0.666675936463772));
#12277=CARTESIAN_POINT('Ctrl Pts',(12.6000020841502,-1.87681550570489,0.668823545630641));
#12278=CARTESIAN_POINT('Ctrl Pts',(12.6000026366798,-1.87471194035196,0.670881441794774));
#12279=CARTESIAN_POINT('Ctrl Pts',(12.6000041308351,-1.86902346102148,0.676446422116204));
#12280=CARTESIAN_POINT('Ctrl Pts',(12.600006461375,-1.86269053299793,0.681293522350018));
#12281=CARTESIAN_POINT('Ctrl Pts',(12.6000072160154,-1.85587841208407,0.685370830723365));
#12282=CARTESIAN_POINT('Ctrl Pts',(12.6000077023835,-1.85148797774957,0.687998669380522));
#12283=CARTESIAN_POINT('Ctrl Pts',(12.6000076405209,-1.84689749427555,0.690306084934615));
#12284=CARTESIAN_POINT('Ctrl Pts',(12.6000070464578,-1.84214500723865,0.692269637845719));
#12285=CARTESIAN_POINT('Ctrl Pts',(12.6000061272438,-1.8347913233911,0.69530790964196));
#12286=CARTESIAN_POINT('Ctrl Pts',(12.6000039197963,-1.82713360831075,0.697490862850871));
#12287=CARTESIAN_POINT('Ctrl Pts',(12.6000021173902,-1.81932000848244,0.698749700991972));
#12288=CARTESIAN_POINT('Ctrl Pts',(12.6000009388424,-1.81421089282246,0.699572823470905));
#12289=CARTESIAN_POINT('Ctrl Pts',(12.6,-1.80903450780073,0.7));
#12290=CARTESIAN_POINT('Ctrl Pts',(12.6,-1.80383022254432,0.7));
#12291=CARTESIAN_POINT('Ctrl Pts',(12.4277899437912,-1.91498765980368,8.1061082099175E-6));
#12292=CARTESIAN_POINT('Ctrl Pts',(12.4185093097394,-1.90440735427916,0.201956437811591));
#12293=CARTESIAN_POINT('Ctrl Pts',(12.4092288296506,-1.89382707230216,0.403904777849331));
#12294=CARTESIAN_POINT('Ctrl Pts',(12.3999485057213,-1.88324681432718,0.605853126346544));
#12295=CARTESIAN_POINT('Ctrl Pts',(11.2514531524596,-1.79377193015415,-0.000335869645892519));
#12296=CARTESIAN_POINT('Ctrl Pts',(11.2440495594319,-1.78319067664719,0.201611894978303));
#12297=CARTESIAN_POINT('Ctrl Pts',(11.2366461029568,-1.77260943823668,0.403559665746509));
#12298=CARTESIAN_POINT('Ctrl Pts',(11.2292427771396,-1.76202821861547,0.605507441576721));
#12299=CARTESIAN_POINT('Ctrl Pts',(10.0755218259154,-1.69940246002113,-0.00057195363688788));
#12300=CARTESIAN_POINT('Ctrl Pts',(10.0699958446785,-1.68882059084335,0.201375418496625));
#12301=CARTESIAN_POINT('Ctrl Pts',(10.0644699805481,-1.67823873210945,0.403322794723726));
#12302=CARTESIAN_POINT('Ctrl Pts',(10.0589442279885,-1.66765688783508,0.605270174140068));
#12303=CARTESIAN_POINT('Ctrl Pts',(8.90001330805802,-1.62424530699552,-0.000736768987564917));
#12304=CARTESIAN_POINT('Ctrl Pts',(8.89636559238287,-1.61366301035882,0.201210329036737));
#12305=CARTESIAN_POINT('Ctrl Pts',(8.89271797406169,-1.60308072296431,0.403157429313698));
#12306=CARTESIAN_POINT('Ctrl Pts',(8.88907045450167,-1.59249844499155,0.605104531878289));
#12307=CARTESIAN_POINT('Ctrl Pts',(8.9000000009702,-1.5932011715731,0.605106081469384));
#12308=CARTESIAN_POINT('Ctrl Pts',(10.0684994345535,-1.66840362346204,0.605023135335662));
#12309=CARTESIAN_POINT('Ctrl Pts',(11.2356615742313,-1.76272273105624,0.604904457271936));
#12310=CARTESIAN_POINT('Ctrl Pts',(12.4,-1.8833055216247,0.604732563714112));
#12311=CARTESIAN_POINT('Ctrl Pts',(12.8889963716306,-1.96391015057091,2.25514051876985E-16));
#12312=CARTESIAN_POINT('Ctrl Pts',(12.8789974396847,-1.95334878321431,0.201594505485581));
#12313=CARTESIAN_POINT('Ctrl Pts',(12.8689986695879,-1.94278744208821,0.403189020401051));
#12314=CARTESIAN_POINT('Ctrl Pts',(12.8590000636394,-1.93222612769726,0.604783544887274));
#12315=CARTESIAN_POINT('Ctrl Pts',(12.792662965057,-1.95339909479377,-3.05216148415599E-5));
#12316=CARTESIAN_POINT('Ctrl Pts',(12.7828174539371,-1.94283764251598,0.201563933758495));
#12317=CARTESIAN_POINT('Ctrl Pts',(12.7729721028852,-1.93227621586528,0.403158398317997));
#12318=CARTESIAN_POINT('Ctrl Pts',(12.7631269141758,-1.92171481533493,0.604752872200892));
#12319=CARTESIAN_POINT('Ctrl Pts',(12.6963322449993,-1.94307475200589,-6.02899321993968E-5));
#12320=CARTESIAN_POINT('Ctrl Pts',(12.6866401583647,-1.93251321719056,0.201534116532542));
#12321=CARTESIAN_POINT('Ctrl Pts',(12.6769482300299,-1.92195170741534,0.403128531945268));
#12322=CARTESIAN_POINT('Ctrl Pts',(12.6672564622455,-1.91139022316239,0.604722956439736));
#12323=CARTESIAN_POINT('Ctrl Pts',(12.6000042264769,-1.9329329264796,-8.93242901516475E-5));
#12324=CARTESIAN_POINT('Ctrl Pts',(12.5904655680581,-1.92237131142302,0.201505034443145));
#12325=CARTESIAN_POINT('Ctrl Pts',(12.5809270661843,-1.91180972083551,0.403099401891705));
#12326=CARTESIAN_POINT('Ctrl Pts',(12.5713887230828,-1.90124815518829,0.604693778185974));
#12327=CARTESIAN_POINT('',(12.8572578715866,-1.93204080633595,0.60466226999893));
#12328=CARTESIAN_POINT('Ctrl Pts',(12.6000000000242,-1.90428042250026,0.604702508168697));
#12329=CARTESIAN_POINT('Ctrl Pts',(12.6857696261193,-1.91338852735451,0.604689390578107));
#12330=CARTESIAN_POINT('Ctrl Pts',(12.7715225733429,-1.92264108900731,0.604675979983877));
#12331=CARTESIAN_POINT('Ctrl Pts',(12.8572578715866,-1.93204080633595,0.60466226999893));
#12332=CARTESIAN_POINT('Ctrl Pts',(12.8572578715866,-1.93204080633595,0.604662269998931));
#12333=CARTESIAN_POINT('Ctrl Pts',(12.867837444884,-1.94266422047353,0.403108198925376));
#12334=CARTESIAN_POINT('Ctrl Pts',(12.8784169445746,-1.95328733374019,0.201554108835025));
#12335=CARTESIAN_POINT('Ctrl Pts',(12.8889963716306,-1.96391015057091,-1.13624387676481E-16));
#12336=CARTESIAN_POINT('Ctrl Pts',(12.4102890066107,-1.7839488953552,0.7));
#12337=CARTESIAN_POINT('Ctrl Pts',(11.2423261062923,-1.6629989551888,0.7));
#12338=CARTESIAN_POINT('Ctrl Pts',(10.0717272052363,-1.56846077660453,0.7));
#12339=CARTESIAN_POINT('Ctrl Pts',(8.89999999999993,-1.49312521822106,0.7));
#12340=CARTESIAN_POINT('Ctrl Pts',(12.4072999778185,-1.81281269415102,0.7));
#12341=CARTESIAN_POINT('Ctrl Pts',(11.2397765858669,-1.69187462084457,0.699998757165067));
#12342=CARTESIAN_POINT('Ctrl Pts',(10.0695527221263,-1.59734372851255,0.700000594792869));
#12343=CARTESIAN_POINT('Ctrl Pts',(8.89814271406455,-1.52201240649035,0.7));
#12344=CARTESIAN_POINT('Ctrl Pts',(12.4021203845267,-1.86282985658401,0.676448561733929));
#12345=CARTESIAN_POINT('Ctrl Pts',(11.2353531757414,-1.74191593276004,0.676505236381959));
#12346=CARTESIAN_POINT('Ctrl Pts',(10.0657879841113,-1.64739716848489,0.676543604639643));
#12347=CARTESIAN_POINT('Ctrl Pts',(8.89492397206972,-1.57207492202614,0.676570833338327));
#12348=CARTESIAN_POINT('Ctrl Pts',(12.400106093269,-1.88228102337346,0.626471792264191));
#12349=CARTESIAN_POINT('Ctrl Pts',(11.2336287644773,-1.76143987438699,0.626617923584012));
#12350=CARTESIAN_POINT('Ctrl Pts',(10.0643137348541,-1.66697079985262,0.626717999675944));
#12351=CARTESIAN_POINT('Ctrl Pts',(8.89366330605793,-1.59168261717615,0.626788336025017));
#12352=CARTESIAN_POINT('Ctrl Pts',(12.4,-1.8833055216247,0.604732563714112));
#12353=CARTESIAN_POINT('Ctrl Pts',(11.2335332423564,-1.7625023138725,0.604904771481731));
#12354=CARTESIAN_POINT('Ctrl Pts',(10.0642324382527,-1.66805889332185,0.605023569028795));
#12355=CARTESIAN_POINT('Ctrl Pts',(8.89359217382714,-1.59278896817116,0.605106535971077));
#12356=CARTESIAN_POINT('Ctrl Pts',(12.400000003046,-1.78288409409898,0.7));
#12357=CARTESIAN_POINT('Ctrl Pts',(11.235451325406,-1.66244391065713,0.7));
#12358=CARTESIAN_POINT('Ctrl Pts',(10.0682865064676,-1.56823955876321,0.7));
#12359=CARTESIAN_POINT('Ctrl Pts',(8.89999999999993,-1.49312521822106,0.7));
#12360=CARTESIAN_POINT('Ctrl Pts',(12.8681436286308,-1.83274446434879,0.7));
#12361=CARTESIAN_POINT('Ctrl Pts',(12.7787800350189,-1.82294762441299,0.7));
#12362=CARTESIAN_POINT('Ctrl Pts',(12.6893984576578,-1.8133105623702,0.7));
#12363=CARTESIAN_POINT('Ctrl Pts',(12.6,-1.80383022254431,0.7));
#12364=CARTESIAN_POINT('Ctrl Pts',(12.8649798835675,-1.86160311979107,0.7));
#12365=CARTESIAN_POINT('Ctrl Pts',(12.7756511334299,-1.85180730951691,0.699999896874207));
#12366=CARTESIAN_POINT('Ctrl Pts',(12.686303642571,-1.84217134991284,0.700000098415946));
#12367=CARTESIAN_POINT('Ctrl Pts',(12.5969393303221,-1.83269196733649,0.7));
#12368=CARTESIAN_POINT('Ctrl Pts',(12.8594976525144,-1.91161025179704,0.676425356750174));
#12369=CARTESIAN_POINT('Ctrl Pts',(12.7702288461641,-1.90181652272411,0.676430055978541));
#12370=CARTESIAN_POINT('Ctrl Pts',(12.6809412203008,-1.89218243450198,0.676434576658958));
#12371=CARTESIAN_POINT('Ctrl Pts',(12.5916356538948,-1.88270499442535,0.67643906321291));
#12372=CARTESIAN_POINT('Ctrl Pts',(12.8573684983393,-1.93103170500986,0.626412260100396));
#12373=CARTESIAN_POINT('Ctrl Pts',(12.7681225846323,-1.92124403769089,0.626424372515079));
#12374=CARTESIAN_POINT('Ctrl Pts',(12.6788572782757,-1.91161594713487,0.626436135819418));
#12375=CARTESIAN_POINT('Ctrl Pts',(12.5895741974899,-1.90214427893475,0.626447702441804));
#12376=CARTESIAN_POINT('Ctrl Pts',(12.8572578715866,-1.93204080633595,0.60466226999893));
#12377=CARTESIAN_POINT('Ctrl Pts',(12.7680127446979,-1.92225628370762,0.604676541242762));
#12378=CARTESIAN_POINT('Ctrl Pts',(12.6787484942245,-1.91263121188365,0.60469048808123));
#12379=CARTESIAN_POINT('Ctrl Pts',(12.5894662143615,-1.9031625467727,0.604704117718382));
#12380=CARTESIAN_POINT('',(12.8681436286308,-1.83274446434879,0.7));
#12381=CARTESIAN_POINT('Ctrl Pts',(12.8681436286308,-1.83274446434879,0.7));
#12382=CARTESIAN_POINT('Ctrl Pts',(12.7787800350189,-1.82294762441299,0.7));
#12383=CARTESIAN_POINT('Ctrl Pts',(12.6893984576578,-1.8133105623702,0.7));
#12384=CARTESIAN_POINT('Ctrl Pts',(12.6,-1.80383022254431,0.7));
#12385=CARTESIAN_POINT('Origin',(12.8681436286308,-1.83274446434879,0.6));
#12386=CARTESIAN_POINT('Origin',(6.87409734069396,-2.22251806091942E-16,
0.7));
#12387=CARTESIAN_POINT('Ctrl Pts',(8.9,1.49312521822106,0.7));
#12388=CARTESIAN_POINT('Ctrl Pts',(10.0682865064677,1.56823955876321,0.7));
#12389=CARTESIAN_POINT('Ctrl Pts',(11.2354513254061,1.66244391065714,0.7));
#12390=CARTESIAN_POINT('Ctrl Pts',(12.4000000030461,1.78288409409899,0.7));
#12391=CARTESIAN_POINT('Origin',(6.87409734069396,-2.22251806091942E-16,
0.7));
#12392=CARTESIAN_POINT('',(12.8681436286308,1.83274446434879,0.7));
#12393=CARTESIAN_POINT('Ctrl Pts',(12.6,1.80383022254432,0.7));
#12394=CARTESIAN_POINT('Ctrl Pts',(12.6893984576578,1.8133105623702,0.7));
#12395=CARTESIAN_POINT('Ctrl Pts',(12.7787800350189,1.82294762441299,0.7));
#12396=CARTESIAN_POINT('Ctrl Pts',(12.8681436286308,1.83274446434879,0.7));
#12397=CARTESIAN_POINT('',(12.8681436286308,1.1,0.7));
#12398=CARTESIAN_POINT('Ctrl Pts',(8.9,1.49312521822106,0.7));
#12399=CARTESIAN_POINT('Ctrl Pts',(10.0717272052363,1.56846077660453,0.7));
#12400=CARTESIAN_POINT('Ctrl Pts',(11.2423261062923,1.6629989551888,0.7));
#12401=CARTESIAN_POINT('Ctrl Pts',(12.4102890066107,1.7839488953552,0.7));
#12402=CARTESIAN_POINT('Ctrl Pts',(8.89814271406461,1.52201240649035,0.7));
#12403=CARTESIAN_POINT('Ctrl Pts',(10.0695527221263,1.59734372851256,0.700000594792869));
#12404=CARTESIAN_POINT('Ctrl Pts',(11.2397765858669,1.69187462084457,0.699998757165067));
#12405=CARTESIAN_POINT('Ctrl Pts',(12.4072999778185,1.81281269415102,0.7));
#12406=CARTESIAN_POINT('Ctrl Pts',(8.89492397206979,1.57207492202615,0.676570833338327));
#12407=CARTESIAN_POINT('Ctrl Pts',(10.0657879841114,1.64739716848489,0.676543604639644));
#12408=CARTESIAN_POINT('Ctrl Pts',(11.2353531757414,1.74191593276004,0.676505236381959));
#12409=CARTESIAN_POINT('Ctrl Pts',(12.4021203845267,1.86282985658401,0.676448561733929));
#12410=CARTESIAN_POINT('Ctrl Pts',(8.89366330605799,1.59168261717616,0.626788336025017));
#12411=CARTESIAN_POINT('Ctrl Pts',(10.0643137348542,1.66697079985262,0.626717999675944));
#12412=CARTESIAN_POINT('Ctrl Pts',(11.2336287644773,1.761439874387,0.626617923584012));
#12413=CARTESIAN_POINT('Ctrl Pts',(12.400106093269,1.88228102337346,0.626471792264191));
#12414=CARTESIAN_POINT('Ctrl Pts',(8.89359217382721,1.59278896817116,0.605106535971077));
#12415=CARTESIAN_POINT('Ctrl Pts',(10.0642324382527,1.66805889332185,0.605023569028795));
#12416=CARTESIAN_POINT('Ctrl Pts',(11.2335332423565,1.7625023138725,0.604904771481731));
#12417=CARTESIAN_POINT('Ctrl Pts',(12.4,1.8833055216247,0.604732563714112));
#12418=CARTESIAN_POINT('Ctrl Pts',(12.4,1.8833055216247,0.604732563714112));
#12419=CARTESIAN_POINT('Ctrl Pts',(11.2356615742313,1.76272273105624,0.604904457271936));
#12420=CARTESIAN_POINT('Ctrl Pts',(10.0684994345535,1.66840362346204,0.605023135335662));
#12421=CARTESIAN_POINT('Ctrl Pts',(8.90000000097019,1.5932011715731,0.605106081469384));
#12422=CARTESIAN_POINT('Ctrl Pts',(8.90001330805765,1.62424530699444,-0.000736768966955875));
#12423=CARTESIAN_POINT('Ctrl Pts',(8.89636559238262,1.6136630103581,0.201210329050476));
#12424=CARTESIAN_POINT('Ctrl Pts',(8.89271797406156,1.60308072296395,0.403157429320568));
#12425=CARTESIAN_POINT('Ctrl Pts',(8.88907045450167,1.59249844499155,0.605104531878289));
#12426=CARTESIAN_POINT('Ctrl Pts',(10.0755218259151,1.69940246002007,-0.000571953616278766));
#12427=CARTESIAN_POINT('Ctrl Pts',(10.0699958446785,1.68882059084265,0.201375418510364));
#12428=CARTESIAN_POINT('Ctrl Pts',(10.0644699805483,1.67823873210911,0.403322794730596));
#12429=CARTESIAN_POINT('Ctrl Pts',(10.0589442279888,1.6676568878351,0.605270174140069));
#12430=CARTESIAN_POINT('Ctrl Pts',(11.2514531524595,1.79377193015312,-0.000335869625283423));
#12431=CARTESIAN_POINT('Ctrl Pts',(11.244049559432,1.78319067664652,0.201611894992042));
#12432=CARTESIAN_POINT('Ctrl Pts',(11.2366461029572,1.77260943823637,0.403559665753379));
#12433=CARTESIAN_POINT('Ctrl Pts',(11.2292427771402,1.76202821861552,0.605507441576721));
#12434=CARTESIAN_POINT('Ctrl Pts',(12.4277899437912,1.9149876598027,8.10612881915578E-6));
#12435=CARTESIAN_POINT('Ctrl Pts',(12.4185093097397,1.90440735427854,0.201956437825331));
#12436=CARTESIAN_POINT('Ctrl Pts',(12.4092288296513,1.89382707230189,0.403904777856201));
#12437=CARTESIAN_POINT('Ctrl Pts',(12.3999485057223,1.88324681432728,0.605853126346545));
#12438=CARTESIAN_POINT('Ctrl Pts',(12.6000042264759,1.9329329264795,-8.93242901520291E-5));
#12439=CARTESIAN_POINT('Ctrl Pts',(12.5904655680574,1.92237131142328,0.201505034436202));
#12440=CARTESIAN_POINT('Ctrl Pts',(12.580927066184,1.91180972083614,0.403099401877819));
#12441=CARTESIAN_POINT('Ctrl Pts',(12.5713887230828,1.90124815518927,0.604693778165146));
#12442=CARTESIAN_POINT('Ctrl Pts',(12.6963322449987,1.94307475200582,-6.02899321996874E-5));
#12443=CARTESIAN_POINT('Ctrl Pts',(12.6866401583644,1.93251321719085,0.201534116525599));
#12444=CARTESIAN_POINT('Ctrl Pts',(12.6769482300299,1.921951707416,0.403128531931383));
#12445=CARTESIAN_POINT('Ctrl Pts',(12.6672564622458,1.91139022316341,0.604722956418908));
#12446=CARTESIAN_POINT('Ctrl Pts',(12.7926629650567,1.95339909479374,-3.05216148420481E-5));
#12447=CARTESIAN_POINT('Ctrl Pts',(12.7828174539371,1.94283764251631,0.201563933751552));
#12448=CARTESIAN_POINT('Ctrl Pts',(12.7729721028855,1.93227621586597,0.403158398304112));
#12449=CARTESIAN_POINT('Ctrl Pts',(12.7631269141765,1.92171481533599,0.604752872180064));
#12450=CARTESIAN_POINT('Ctrl Pts',(12.8889963716306,1.96391015057091,-1.66533453693773E-16));
#12451=CARTESIAN_POINT('Ctrl Pts',(12.878997439685,1.95334878321468,0.201594505478638));
#12452=CARTESIAN_POINT('Ctrl Pts',(12.8689986695886,1.94278744208894,0.403189020387166));
#12453=CARTESIAN_POINT('Ctrl Pts',(12.8590000636404,1.93222612769835,0.604783544866446));
#12454=CARTESIAN_POINT('',(12.8572578715866,1.93204080633595,0.60466226999893));
#12455=CARTESIAN_POINT('Ctrl Pts',(12.8889963716306,1.96391015057091,-3.88144377749811E-17));
#12456=CARTESIAN_POINT('Ctrl Pts',(12.8784169445746,1.95328733374019,0.201554108835021));
#12457=CARTESIAN_POINT('Ctrl Pts',(12.867837444884,1.94266422047353,0.403108198925375));
#12458=CARTESIAN_POINT('Ctrl Pts',(12.8572578715866,1.93204080633595,0.604662269998929));
#12459=CARTESIAN_POINT('Ctrl Pts',(12.8572578715866,1.93204080633595,0.60466226999893));
#12460=CARTESIAN_POINT('Ctrl Pts',(12.7715225733429,1.92264108900731,0.604675979983877));
#12461=CARTESIAN_POINT('Ctrl Pts',(12.6857696261193,1.91338852735451,0.604689390578107));
#12462=CARTESIAN_POINT('Ctrl Pts',(12.6000000000242,1.90428042250026,0.604702508168697));
#12463=CARTESIAN_POINT('Origin',(8.7,1.68851851851852,0.));
#12464=CARTESIAN_POINT('',(8.7,-1.5805153611151,0.605119933308333));
#12465=CARTESIAN_POINT('Ctrl Pts',(8.7,-1.5805153611151,0.605119933308333));
#12466=CARTESIAN_POINT('Ctrl Pts',(8.7,-1.58569938832865,0.504197823486131));
#12467=CARTESIAN_POINT('Ctrl Pts',(8.7,-1.59088373519313,0.403275164205241));
#12468=CARTESIAN_POINT('Ctrl Pts',(8.7,-1.60124586355191,0.201568897935389));
#12469=CARTESIAN_POINT('Ctrl Pts',(8.7,-1.60642370224807,0.10078416210737));
#12470=CARTESIAN_POINT('Ctrl Pts',(8.7,-1.61160179736194,0.));
#12471=CARTESIAN_POINT('',(8.7,-1.48045180431786,0.7));
#12472=CARTESIAN_POINT('Ctrl Pts',(8.70000000036779,-1.48045180452391,0.7));
#12473=CARTESIAN_POINT('Ctrl Pts',(8.70000000202598,-1.48836706478042,0.699999999180279));
#12474=CARTESIAN_POINT('Ctrl Pts',(8.70000127066624,-1.49622113223642,0.699007614827928));
#12475=CARTESIAN_POINT('Ctrl Pts',(8.70000237141531,-1.50387364922569,0.697121884028934));
#12476=CARTESIAN_POINT('Ctrl Pts',(8.70000291188189,-1.50763102664002,0.696195992283305));
#12477=CARTESIAN_POINT('Ctrl Pts',(8.70000341240591,-1.51133980954515,0.695053883793301));
#12478=CARTESIAN_POINT('Ctrl Pts',(8.70000377175886,-1.51498230649063,0.693702880475192));
#12479=CARTESIAN_POINT('Ctrl Pts',(8.70000450976793,-1.52246296255016,0.690928302676144));
#12480=CARTESIAN_POINT('Ctrl Pts',(8.70000452394134,-1.52958344744078,0.687306123577328));
#12481=CARTESIAN_POINT('Ctrl Pts',(8.70000379461986,-1.53619834892264,0.682919715776694));
#12482=CARTESIAN_POINT('Ctrl Pts',(8.70000333219987,-1.54039247012311,0.680138551763745));
#12483=CARTESIAN_POINT('Ctrl Pts',(8.70000258238552,-1.54438316197938,0.67704909562189));
#12484=CARTESIAN_POINT('Ctrl Pts',(8.70000192913237,-1.54812716280968,0.67366362845569));
#12485=CARTESIAN_POINT('Ctrl Pts',(8.70000138361353,-1.55125370412533,0.670836491537814));
#12486=CARTESIAN_POINT('Ctrl Pts',(8.70000090341281,-1.55418891097064,0.66782012731024));
#12487=CARTESIAN_POINT('Ctrl Pts',(8.7000009033621,-1.55691103280728,0.664625500020687));
#12488=CARTESIAN_POINT('Ctrl Pts',(8.7000009032669,-1.56202159382457,0.658627848677152));
#12489=CARTESIAN_POINT('Ctrl Pts',(8.70000241148087,-1.56638404855443,0.652003279246098));
#12490=CARTESIAN_POINT('Ctrl Pts',(8.70000292788623,-1.5699383402149,0.64491699469699));
#12491=CARTESIAN_POINT('Ctrl Pts',(8.70000298354275,-1.57032141040405,0.644153257609021));
#12492=CARTESIAN_POINT('Ctrl Pts',(8.70000303046442,-1.57069504840788,0.643384135640712));
#12493=CARTESIAN_POINT('Ctrl Pts',(8.70000306761332,-1.57105914547653,0.642609822781892));
#12494=CARTESIAN_POINT('Ctrl Pts',(8.70000341208914,-1.57443535963509,0.635429742901602));
#12495=CARTESIAN_POINT('Ctrl Pts',(8.70000263566904,-1.57695592401075,0.627888404173009));
#12496=CARTESIAN_POINT('Ctrl Pts',(8.70000151703179,-1.57856725066757,0.620153930269154));
#12497=CARTESIAN_POINT('Ctrl Pts',(8.70000080174396,-1.57959757782623,0.615208292159515));
#12498=CARTESIAN_POINT('Ctrl Pts',(8.7,-1.58025528705454,0.610183028431161));
#12499=CARTESIAN_POINT('Ctrl Pts',(8.7,-1.5805153611151,0.605119933308333));
#12500=CARTESIAN_POINT('',(8.7,1.48045180431904,0.7));
#12501=CARTESIAN_POINT('',(8.7,0.844259259259259,0.7));
#12502=CARTESIAN_POINT('',(8.7,1.5805153611151,0.605119933308333));
#12503=CARTESIAN_POINT('Ctrl Pts',(8.7,1.5805153611151,0.605119933308333));
#12504=CARTESIAN_POINT('Ctrl Pts',(8.7,1.58010890623597,0.61303275518587));
#12505=CARTESIAN_POINT('Ctrl Pts',(8.70000179355525,1.57873376841273,0.620855553142259));
#12506=CARTESIAN_POINT('Ctrl Pts',(8.7000025961206,1.5764741717406,0.62842799710221));
#12507=CARTESIAN_POINT('Ctrl Pts',(8.70000304562639,1.57520860278123,0.632669218617747));
#12508=CARTESIAN_POINT('Ctrl Pts',(8.70000324668712,1.57366457852079,0.636831947144834));
#12509=CARTESIAN_POINT('Ctrl Pts',(8.70000313318341,1.57185009366145,0.640886032861668));
#12510=CARTESIAN_POINT('Ctrl Pts',(8.70000293045856,1.56860930815545,0.648126888117959));
#12511=CARTESIAN_POINT('Ctrl Pts',(8.70000158438082,1.56454425420738,0.654942317779106));
#12512=CARTESIAN_POINT('Ctrl Pts',(8.70000106269264,1.55971945710293,0.661169479919421));
#12513=CARTESIAN_POINT('Ctrl Pts',(8.70000096439252,1.55881033523018,0.662342845179011));
#12514=CARTESIAN_POINT('Ctrl Pts',(8.70000090351839,1.55787410801649,0.663495254390581));
#12515=CARTESIAN_POINT('Ctrl Pts',(8.70000090409683,1.55691103285321,0.664625500020665));
#12516=CARTESIAN_POINT('Ctrl Pts',(8.70000090523835,1.55501044337284,0.666855993586132));
#12517=CARTESIAN_POINT('Ctrl Pts',(8.70000114361209,1.55300532702719,0.669000219206223));
#12518=CARTESIAN_POINT('Ctrl Pts',(8.70000146777886,1.55090303951829,0.671054438207787));
#12519=CARTESIAN_POINT('Ctrl Pts',(8.70000234447876,1.54521746205001,0.676610015749294));
#12520=CARTESIAN_POINT('Ctrl Pts',(8.70000370702799,1.53888821826629,0.681447385411957));
#12521=CARTESIAN_POINT('Ctrl Pts',(8.70000415375638,1.53207947242364,0.685512859850771));
#12522=CARTESIAN_POINT('Ctrl Pts',(8.70000443876751,1.52773551673798,0.688106618115728));
#12523=CARTESIAN_POINT('Ctrl Pts',(8.70000441165582,1.52319541573235,0.690385508075002));
#12524=CARTESIAN_POINT('Ctrl Pts',(8.70000407315693,1.51849599021366,0.692326230693156));
#12525=CARTESIAN_POINT('Ctrl Pts',(8.70000354533424,1.51116815716702,0.695352407250086));
#12526=CARTESIAN_POINT('Ctrl Pts',(8.70000225790696,1.50353761203248,0.697524030080351));
#12527=CARTESIAN_POINT('Ctrl Pts',(8.70000121423997,1.49575164755759,0.698771658000832));
#12528=CARTESIAN_POINT('Ctrl Pts',(8.70000053774506,1.49070486028667,0.699580358416591));
#12529=CARTESIAN_POINT('Ctrl Pts',(8.70000000144466,1.48559217323052,0.699999999467653));
#12530=CARTESIAN_POINT('Ctrl Pts',(8.70000000036779,1.48045180452391,0.7));
#12531=CARTESIAN_POINT('Ctrl Pts',(8.7,1.61160179736194,0.));
#12532=CARTESIAN_POINT('Ctrl Pts',(8.7,1.60642368739695,0.100784451162898));
#12533=CARTESIAN_POINT('Ctrl Pts',(8.7,1.60124583384883,0.201569476094892));
#12534=CARTESIAN_POINT('Ctrl Pts',(8.7,1.59088370548997,0.403275742430776));
#12535=CARTESIAN_POINT('Ctrl Pts',(8.7,1.58569937347746,0.504198112607714));
#12536=CARTESIAN_POINT('Ctrl Pts',(8.7,1.5805153611151,0.605119933308333));
#12537=CARTESIAN_POINT('Ctrl Pts',(8.7100201910492,-1.61222456240079,1.33887903992595E-6));
#12538=CARTESIAN_POINT('Ctrl Pts',(8.70667727354472,-1.60164608969543,0.201874135619687));
#12539=CARTESIAN_POINT('Ctrl Pts',(8.70333445073708,-1.59106762573893,0.40374693439627));
#12540=CARTESIAN_POINT('Ctrl Pts',(8.69999172399519,-1.58048917070122,0.605619735240497));
#12541=CARTESIAN_POINT('Ctrl Pts',(7.30266630830786,-1.52469223633113,-0.000186944012493601));
#12542=CARTESIAN_POINT('Ctrl Pts',(7.3015714609838,-1.51411327886182,0.201685539385837));
#12543=CARTESIAN_POINT('Ctrl Pts',(7.30047669312962,-1.50353432123569,0.403558023359813));
#12544=CARTESIAN_POINT('Ctrl Pts',(7.2993819983171,-1.49295537435081,0.605430507723141));
#12545=CARTESIAN_POINT('Ctrl Pts',(5.89591889571946,-1.46411055243784,-0.000276130330627546));
#12546=CARTESIAN_POINT('Ctrl Pts',(5.8970730573458,-1.45353136553189,0.201596203763285));
#12547=CARTESIAN_POINT('Ctrl Pts',(5.89822728315403,-1.44295217665945,0.403468537584815));
#12548=CARTESIAN_POINT('Ctrl Pts',(5.89938156763751,-1.43237299696387,0.60534087113472));
#12549=CARTESIAN_POINT('Ctrl Pts',(4.48978738186403,-1.41740792524342,-0.000330195618103912));
#12550=CARTESIAN_POINT('Ctrl Pts',(4.49319153668887,-1.4068286019831,0.201542048187911));
#12551=CARTESIAN_POINT('Ctrl Pts',(4.49659574248722,-1.39624928130228,0.403414291272231));
#12552=CARTESIAN_POINT('Ctrl Pts',(4.5,-1.3856699632509,0.605286533625018));
#12553=CARTESIAN_POINT('Ctrl Pts',(4.50000000014037,-1.38566996330298,0.605286533623957));
#12554=CARTESIAN_POINT('Ctrl Pts',(5.90109530155974,-1.43243455365708,0.605259331490037));
#12555=CARTESIAN_POINT('Ctrl Pts',(7.30150776148394,-1.49309969195427,0.605214402664297));
#12556=CARTESIAN_POINT('Ctrl Pts',(8.7,-1.5805153611151,0.605119933308333));
#12557=CARTESIAN_POINT('Ctrl Pts',(8.7062300060629,-1.48084102486261,0.7));
#12558=CARTESIAN_POINT('Ctrl Pts',(7.30535837857749,-1.39328148786737,0.7));
#12559=CARTESIAN_POINT('Ctrl Pts',(5.90286553803659,-1.3325543763676,0.7));
#12560=CARTESIAN_POINT('Ctrl Pts',(4.5,-1.28575421950843,0.7));
#12561=CARTESIAN_POINT('Ctrl Pts',(8.7044244076592,-1.50972892972339,0.7));
#12562=CARTESIAN_POINT('Ctrl Pts',(7.30392377861185,-1.42217417124324,0.699999322371676));
#12563=CARTESIAN_POINT('Ctrl Pts',(5.90170976758769,-1.36144968116949,0.700000194339816));
#12564=CARTESIAN_POINT('Ctrl Pts',(4.49903600403804,-1.314650633636,0.7));
#12565=CARTESIAN_POINT('Ctrl Pts',(8.70129509098077,-1.55979510296572,0.676577193851887));
#12566=CARTESIAN_POINT('Ctrl Pts',(7.30143307762773,-1.47225060169427,0.676608218952397));
#12567=CARTESIAN_POINT('Ctrl Pts',(5.89970879741633,-1.41153023905743,0.676622651488038));
#12568=CARTESIAN_POINT('Ctrl Pts',(4.49736521340071,-1.36473368385825,0.676631564755462));
#12569=CARTESIAN_POINT('Ctrl Pts',(8.70006933407556,-1.57940608001781,0.626799670546273));
#12570=CARTESIAN_POINT('Ctrl Pts',(7.3004573192207,-1.49190036240803,0.626879818917698));
#12571=CARTESIAN_POINT('Ctrl Pts',(5.89892183391985,-1.43119871194172,0.62691759730524));
#12572=CARTESIAN_POINT('Ctrl Pts',(4.49670869913724,-1.38441313147668,0.626940642142451));
#12573=CARTESIAN_POINT('Ctrl Pts',(8.7,-1.5805153611151,0.605119933308333));
#12574=CARTESIAN_POINT('Ctrl Pts',(7.30039998287682,-1.49303044794594,0.605214477495697));
#12575=CARTESIAN_POINT('Ctrl Pts',(5.89887670103551,-1.4323384618751,0.605259402637312));
#12576=CARTESIAN_POINT('Ctrl Pts',(4.49667047719213,-1.38555885946567,0.605286598232956));
#12577=CARTESIAN_POINT('Ctrl Pts',(8.70000000036771,-1.48045180452391,0.7));
#12578=CARTESIAN_POINT('Ctrl Pts',(7.30120024114866,-1.39310147361351,0.7));
#12579=CARTESIAN_POINT('Ctrl Pts',(5.90078591724148,-1.332484999384,0.7));
#12580=CARTESIAN_POINT('Ctrl Pts',(4.5,-1.28575421950843,0.7));
#12581=CARTESIAN_POINT('Origin',(6.87409734069396,-2.22251806091942E-16,
0.7));
#12582=CARTESIAN_POINT('Ctrl Pts',(4.5,1.28575421950843,0.7));
#12583=CARTESIAN_POINT('Ctrl Pts',(5.9007859172415,1.332484999384,0.7));
#12584=CARTESIAN_POINT('Ctrl Pts',(7.30120024114871,1.39310147361351,0.7));
#12585=CARTESIAN_POINT('Ctrl Pts',(8.70000000036779,1.48045180452391,0.7));
#12586=CARTESIAN_POINT('Ctrl Pts',(4.5,1.28575421950843,0.7));
#12587=CARTESIAN_POINT('Ctrl Pts',(5.90286553803659,1.3325543763676,0.7));
#12588=CARTESIAN_POINT('Ctrl Pts',(7.30535837857749,1.39328148786737,0.7));
#12589=CARTESIAN_POINT('Ctrl Pts',(8.7062300060629,1.48084102486261,0.7));
#12590=CARTESIAN_POINT('Ctrl Pts',(4.49903600403804,1.314650633636,0.7));
#12591=CARTESIAN_POINT('Ctrl Pts',(5.90170976758769,1.36144968116949,0.700000194339816));
#12592=CARTESIAN_POINT('Ctrl Pts',(7.30392377861185,1.42217417124324,0.699999322371676));
#12593=CARTESIAN_POINT('Ctrl Pts',(8.7044244076592,1.50972892972339,0.7));
#12594=CARTESIAN_POINT('Ctrl Pts',(4.49736521340071,1.36473368385825,0.676631564755462));
#12595=CARTESIAN_POINT('Ctrl Pts',(5.89970879741633,1.41153023905743,0.676622651488038));
#12596=CARTESIAN_POINT('Ctrl Pts',(7.30143307762774,1.47225060169427,0.676608218952397));
#12597=CARTESIAN_POINT('Ctrl Pts',(8.70129509098078,1.55979510296572,0.676577193851887));
#12598=CARTESIAN_POINT('Ctrl Pts',(4.49670869913724,1.38441313147668,0.626940642142451));
#12599=CARTESIAN_POINT('Ctrl Pts',(5.89892183391985,1.43119871194172,0.626917597305239));
#12600=CARTESIAN_POINT('Ctrl Pts',(7.3004573192207,1.49190036240803,0.626879818917698));
#12601=CARTESIAN_POINT('Ctrl Pts',(8.70006933407556,1.57940608001781,0.626799670546273));
#12602=CARTESIAN_POINT('Ctrl Pts',(4.49667047719213,1.38555885946567,0.605286598232956));
#12603=CARTESIAN_POINT('Ctrl Pts',(5.89887670103551,1.4323384618751,0.605259402637312));
#12604=CARTESIAN_POINT('Ctrl Pts',(7.30039998287682,1.49303044794594,0.605214477495697));
#12605=CARTESIAN_POINT('Ctrl Pts',(8.7,1.5805153611151,0.605119933308333));
#12606=CARTESIAN_POINT('Ctrl Pts',(8.7,1.5805153611151,0.605119933308333));
#12607=CARTESIAN_POINT('Ctrl Pts',(7.30150776148394,1.49309969195427,0.605214402664297));
#12608=CARTESIAN_POINT('Ctrl Pts',(5.90109530155974,1.43243455365708,0.605259331490037));
#12609=CARTESIAN_POINT('Ctrl Pts',(4.50000000014037,1.38566996330298,0.605286533623957));
#12610=CARTESIAN_POINT('Ctrl Pts',(4.48978738186405,1.41740792524342,-0.00033019561810394));
#12611=CARTESIAN_POINT('Ctrl Pts',(4.49319153668889,1.40682860198312,0.201542048187577));
#12612=CARTESIAN_POINT('Ctrl Pts',(4.49659574248723,1.39624928130232,0.403414291271564));
#12613=CARTESIAN_POINT('Ctrl Pts',(4.5,1.38566996325095,0.605286533624017));
#12614=CARTESIAN_POINT('Ctrl Pts',(5.89591889571947,1.46411055243784,-0.000276130330627574));
#12615=CARTESIAN_POINT('Ctrl Pts',(5.89707305734581,1.45353136553191,0.201596203762952));
#12616=CARTESIAN_POINT('Ctrl Pts',(5.89822728315404,1.44295217665948,0.403468537584147));
#12617=CARTESIAN_POINT('Ctrl Pts',(5.89938156763751,1.43237299696393,0.605340871133719));
#12618=CARTESIAN_POINT('Ctrl Pts',(7.30266630830786,1.52469223633113,-0.000186944012493549));
#12619=CARTESIAN_POINT('Ctrl Pts',(7.3015714609838,1.51411327886184,0.201685539385503));
#12620=CARTESIAN_POINT('Ctrl Pts',(7.30047669312963,1.50353432123572,0.403558023359145));
#12621=CARTESIAN_POINT('Ctrl Pts',(7.29938199831711,1.49295537435086,0.60543050772214));
#12622=CARTESIAN_POINT('Ctrl Pts',(8.7100201910492,1.61222456240079,1.33887903989646E-6));
#12623=CARTESIAN_POINT('Ctrl Pts',(8.70667727354472,1.60164608969545,0.201874135619353));
#12624=CARTESIAN_POINT('Ctrl Pts',(8.7033344507371,1.59106762573896,0.403746934395602));
#12625=CARTESIAN_POINT('Ctrl Pts',(8.6999917239952,1.58048917070127,0.605619735239495));
#12626=CARTESIAN_POINT('Origin',(4.3,1.48481481481482,0.));
#12627=CARTESIAN_POINT('',(4.3,-1.37908752581626,0.605290299758539));
#12628=CARTESIAN_POINT('Ctrl Pts',(4.3,-1.37908752581626,0.605290299758539));
#12629=CARTESIAN_POINT('Ctrl Pts',(4.3,-1.38444464017247,0.504222347694443));
#12630=CARTESIAN_POINT('Ctrl Pts',(4.3,-1.38980163214303,0.403154389143214));
#12631=CARTESIAN_POINT('Ctrl Pts',(4.3,-1.40049562949383,0.201390955816302));
#12632=CARTESIAN_POINT('Ctrl Pts',(4.3,-1.40583263576898,0.100695481088992));
#12633=CARTESIAN_POINT('Ctrl Pts',(4.3,-1.41116952203211,0.));
#12634=CARTESIAN_POINT('Ctrl Pts',(4.30000000005992,-1.27917501058303,0.7));
#12635=CARTESIAN_POINT('Ctrl Pts',(4.30000000048661,-1.28708628524264,0.699999999884766));
#12636=CARTESIAN_POINT('Ctrl Pts',(4.30000064978116,-1.29493415608545,0.69900616264686));
#12637=CARTESIAN_POINT('Ctrl Pts',(4.30000121018478,-1.30257825621016,0.697119208693397));
#12638=CARTESIAN_POINT('Ctrl Pts',(4.30000152558655,-1.30688044586137,0.696057208766858));
#12639=CARTESIAN_POINT('Ctrl Pts',(4.30000181105247,-1.31111814675806,0.694711271736901));
#12640=CARTESIAN_POINT('Ctrl Pts',(4.30000199036827,-1.31526464671957,0.693092387263961));
#12641=CARTESIAN_POINT('Ctrl Pts',(4.30000231141323,-1.32268849323592,0.690193954859197));
#12642=CARTESIAN_POINT('Ctrl Pts',(4.30000222777046,-1.32973966400828,0.686455190804221));
#12643=CARTESIAN_POINT('Ctrl Pts',(4.30000179417102,-1.33627196700415,0.681957645816867));
#12644=CARTESIAN_POINT('Ctrl Pts',(4.30000155535849,-1.33986974800182,0.679480543652151));
#12645=CARTESIAN_POINT('Ctrl Pts',(4.30000121902461,-1.34330986828215,0.67677238407294));
#12646=CARTESIAN_POINT('Ctrl Pts',(4.30000092191081,-1.34656397897095,0.673841242448196));
#12647=CARTESIAN_POINT('Ctrl Pts',(4.30000063243573,-1.34973442737118,0.670985459666446));
#12648=CARTESIAN_POINT('Ctrl Pts',(4.30000037658882,-1.35270906921767,0.667935271966333));
#12649=CARTESIAN_POINT('Ctrl Pts',(4.30000037869864,-1.35546536049262,0.66470214425512));
#12650=CARTESIAN_POINT('Ctrl Pts',(4.30000038260995,-1.36057515211559,0.658708362304413));
#12651=CARTESIAN_POINT('Ctrl Pts',(4.30000117797282,-1.36493744806469,0.652087250959406));
#12652=CARTESIAN_POINT('Ctrl Pts',(4.30000145944905,-1.36849285270534,0.645004510397983));
#12653=CARTESIAN_POINT('Ctrl Pts',(4.30000148826005,-1.36885677248754,0.644279543857467));
#12654=CARTESIAN_POINT('Ctrl Pts',(4.30000151299237,-1.36921219826683,0.643549721050429));
#12655=CARTESIAN_POINT('Ctrl Pts',(4.30000153317099,-1.36955903781249,0.642815208524159));
#12656=CARTESIAN_POINT('Ctrl Pts',(4.30000173031152,-1.37294758118467,0.635639188419686));
#12657=CARTESIAN_POINT('Ctrl Pts',(4.30000134819424,-1.37548140076902,0.628100134775109));
#12658=CARTESIAN_POINT('Ctrl Pts',(4.30000077902196,-1.37710733725971,0.620366659714886));
#12659=CARTESIAN_POINT('Ctrl Pts',(4.30000041405338,-1.37814993145247,0.615407747584041));
#12660=CARTESIAN_POINT('Ctrl Pts',(4.3,-1.37881837002099,0.610368224776708));
#12661=CARTESIAN_POINT('Ctrl Pts',(4.3,-1.37908752581626,0.605290299758539));
#12662=CARTESIAN_POINT('',(4.3,1.37908752581626,0.605290299758539));
#12663=CARTESIAN_POINT('Ctrl Pts',(4.3,1.37908752581626,0.605290299758539));
#12664=CARTESIAN_POINT('Ctrl Pts',(4.3,1.37866806817032,0.613203837240499));
#12665=CARTESIAN_POINT('Ctrl Pts',(4.30000092021544,1.37728139671899,0.621026590428679));
#12666=CARTESIAN_POINT('Ctrl Pts',(4.30000132151137,1.37501133257008,0.628597948954885));
#12667=CARTESIAN_POINT('Ctrl Pts',(4.30000154544343,1.37374458621782,0.632822935636113));
#12668=CARTESIAN_POINT('Ctrl Pts',(4.30000164013187,1.37220176226583,0.636969676056352));
#12669=CARTESIAN_POINT('Ctrl Pts',(4.30000157305315,1.37039070587839,0.641008268098125));
#12670=CARTESIAN_POINT('Ctrl Pts',(4.30000145288191,1.36714620633991,0.648243387946652));
#12671=CARTESIAN_POINT('Ctrl Pts',(4.30000073948134,1.36307905360626,0.655053358422861));
#12672=CARTESIAN_POINT('Ctrl Pts',(4.3000004635866,1.35825284513469,0.661274801567968));
#12673=CARTESIAN_POINT('Ctrl Pts',(4.30000041199046,1.35735027731582,0.662438297592388));
#12674=CARTESIAN_POINT('Ctrl Pts',(4.30000037986005,1.35642103364291,0.663581140343808));
#12675=CARTESIAN_POINT('Ctrl Pts',(4.30000037943224,1.35546536051643,0.664702144255114));
#12676=CARTESIAN_POINT('Ctrl Pts',(4.300000378582,1.3535659898678,0.666930104702213));
#12677=CARTESIAN_POINT('Ctrl Pts',(4.3000005018795,1.35156225525783,0.669071850305581));
#12678=CARTESIAN_POINT('Ctrl Pts',(4.30000067038034,1.34946148384904,0.671123623013939));
#12679=CARTESIAN_POINT('Ctrl Pts',(4.30000112630012,1.34377733881547,0.676675190215126));
#12680=CARTESIAN_POINT('Ctrl Pts',(4.30000183907902,1.33744971106208,0.68150833207295));
#12681=CARTESIAN_POINT('Ctrl Pts',(4.30000208123143,1.33064243458576,0.685568782013219));
#12682=CARTESIAN_POINT('Ctrl Pts',(4.30000223513396,1.3263159977886,0.688149444058562));
#12683=CARTESIAN_POINT('Ctrl Pts',(4.3000022300233,1.32179485563522,0.690417305529342));
#12684=CARTESIAN_POINT('Ctrl Pts',(4.30000206344016,1.31711540146937,0.692349146556373));
#12685=CARTESIAN_POINT('Ctrl Pts',(4.3000018029167,1.30979708846622,0.695370400063095));
#12686=CARTESIAN_POINT('Ctrl Pts',(4.30000114702936,1.30217656646843,0.69753735975804));
#12687=CARTESIAN_POINT('Ctrl Pts',(4.3000006156201,1.29440092269557,0.69878042986007));
#12688=CARTESIAN_POINT('Ctrl Pts',(4.30000027236218,1.28937833178082,0.699583377215073));
#12689=CARTESIAN_POINT('Ctrl Pts',(4.30000000033581,1.28429042584107,0.69999999992549));
#12690=CARTESIAN_POINT('Ctrl Pts',(4.30000000005992,1.27917501058303,0.7));
#12691=CARTESIAN_POINT('Ctrl Pts',(4.3,1.41116952203211,0.));
#12692=CARTESIAN_POINT('Ctrl Pts',(4.3,1.40583262613343,0.100695662891028));
#12693=CARTESIAN_POINT('Ctrl Pts',(4.3,1.40049561022223,0.201391319421434));
#12694=CARTESIAN_POINT('Ctrl Pts',(4.3,1.38980161287056,0.403154752748307));
#12695=CARTESIAN_POINT('Ctrl Pts',(4.3,1.38444463053604,0.504222529496425));
#12696=CARTESIAN_POINT('Ctrl Pts',(4.3,1.37908752581626,0.605290299758539));
#12697=CARTESIAN_POINT('Ctrl Pts',(4.3,-1.41116952203217,-1.08233907947231E-12));
#12698=CARTESIAN_POINT('Ctrl Pts',(4.30370667985561,-1.40059355144761,0.201807922462111));
#12699=CARTESIAN_POINT('Ctrl Pts',(4.30741340932898,-1.39001758331341,0.403615844144917));
#12700=CARTESIAN_POINT('Ctrl Pts',(4.31112018914117,-1.37944161767694,0.605423765036612));
#12701=CARTESIAN_POINT('Ctrl Pts',(3.22410085073145,-1.37636920007795,-3.90459529712038E-5));
#12702=CARTESIAN_POINT('Ctrl Pts',(3.2295286994181,-1.36579313421488,0.201768811380596));
#12703=CARTESIAN_POINT('Ctrl Pts',(3.23495659078338,-1.35521706809947,0.403576667516588));
#12704=CARTESIAN_POINT('Ctrl Pts',(3.24038452463065,-1.34464100578453,0.605384522622892));
#12705=CARTESIAN_POINT('Ctrl Pts',(2.14856196511704,-1.34935185539723,-5.92140864038068E-5));
#12706=CARTESIAN_POINT('Ctrl Pts',(2.15571155670467,-1.33877574824886,0.201748609775608));
#12707=CARTESIAN_POINT('Ctrl Pts',(2.16286118630165,-1.32819964054015,0.403556432267456));
#12708=CARTESIAN_POINT('Ctrl Pts',(2.17001085376486,-1.31762353633116,0.605364253566666));
#12709=CARTESIAN_POINT('Ctrl Pts',(1.073384157387,-1.32427529283232,-8.86713468529234E-5));
#12710=CARTESIAN_POINT('Ctrl Pts',(1.08225606990756,-1.31369916974321,0.201719104822629));
#12711=CARTESIAN_POINT('Ctrl Pts',(1.09112801825726,-1.30312304798914,0.403526879488275));
#12712=CARTESIAN_POINT('Ctrl Pts',(1.10000000295732,-1.29254692759565,0.605334652628532));
#12713=CARTESIAN_POINT('Ctrl Pts',(1.10000000298281,-1.29254692760111,0.605334652628557));
#12714=CARTESIAN_POINT('Ctrl Pts',(2.16694388170712,-1.31755402957363,0.605319894542965));
#12715=CARTESIAN_POINT('Ctrl Pts',(3.23367147240841,-1.34448060345116,0.605309774863278));
#12716=CARTESIAN_POINT('Ctrl Pts',(4.3,-1.37908752581626,0.605290299758539));
#12717=CARTESIAN_POINT('Ctrl Pts',(4.30323908112369,-1.2792801058419,0.7));
#12718=CARTESIAN_POINT('Ctrl Pts',(3.23565147654712,-1.24463335454069,0.7));
#12719=CARTESIAN_POINT('Ctrl Pts',(2.1678436779024,-1.21768649131741,0.7));
#12720=CARTESIAN_POINT('Ctrl Pts',(1.09999999999999,-1.19266190204553,0.7));
#12721=CARTESIAN_POINT('Ctrl Pts',(4.30230129178181,-1.30817667592415,0.7));
#12722=CARTESIAN_POINT('Ctrl Pts',(3.23485320804887,-1.27353066282864,0.699999860738333));
#12723=CARTESIAN_POINT('Ctrl Pts',(2.16713169816659,-1.24658393122273,0.700000105496227));
#12724=CARTESIAN_POINT('Ctrl Pts',(1.0993228455422,-1.22155728565617,0.7));
#12725=CARTESIAN_POINT('Ctrl Pts',(4.30067574076257,-1.35826558912881,0.676637683834297));
#12726=CARTESIAN_POINT('Ctrl Pts',(3.23346787205668,-1.32362126434549,0.676644071225102));
#12727=CARTESIAN_POINT('Ctrl Pts',(2.16589795861771,-1.29667457247055,0.676647306834711));
#12728=CARTESIAN_POINT('Ctrl Pts',(1.09814906228501,-1.27164470234869,0.676652147774997));
#12729=CARTESIAN_POINT('Ctrl Pts',(4.30003720890047,-1.37794098943329,0.626943772371838));
#12730=CARTESIAN_POINT('Ctrl Pts',(3.23292426239396,-1.34330449078822,0.626960286972675));
#12731=CARTESIAN_POINT('Ctrl Pts',(2.16541285690349,-1.31636171257899,0.6269687859393));
#12732=CARTESIAN_POINT('Ctrl Pts',(1.09768760301306,-1.29133598921902,0.626981304916489));
#12733=CARTESIAN_POINT('Ctrl Pts',(4.3,-1.37908752581626,0.605290299758539));
#12734=CARTESIAN_POINT('Ctrl Pts',(3.23289209128077,-1.34445530919946,0.605309789097661));
#12735=CARTESIAN_POINT('Ctrl Pts',(2.16538453588699,-1.31751467232976,0.605319909330946));
#12736=CARTESIAN_POINT('Ctrl Pts',(1.09766050997011,-1.29249209748956,0.605334684996117));
#12737=CARTESIAN_POINT('Ctrl Pts',(1.09999999999999,1.19266190204553,0.7));
#12738=CARTESIAN_POINT('Ctrl Pts',(2.1678436779024,1.21768649131741,0.7));
#12739=CARTESIAN_POINT('Ctrl Pts',(3.23565147654712,1.24463335454069,0.7));
#12740=CARTESIAN_POINT('Ctrl Pts',(4.30323908112369,1.2792801058419,0.7));
#12741=CARTESIAN_POINT('Ctrl Pts',(1.0993228455422,1.22155728565617,0.7));
#12742=CARTESIAN_POINT('Ctrl Pts',(2.16713169816659,1.24658393122273,0.700000105496227));
#12743=CARTESIAN_POINT('Ctrl Pts',(3.23485320804887,1.27353066282864,0.699999860738333));
#12744=CARTESIAN_POINT('Ctrl Pts',(4.30230129178181,1.30817667592415,0.7));
#12745=CARTESIAN_POINT('Ctrl Pts',(1.09814906228501,1.27164470234869,0.676652147774997));
#12746=CARTESIAN_POINT('Ctrl Pts',(2.16589795861771,1.29667457247055,0.676647306834711));
#12747=CARTESIAN_POINT('Ctrl Pts',(3.23346787205668,1.32362126434549,0.676644071225102));
#12748=CARTESIAN_POINT('Ctrl Pts',(4.30067574076257,1.35826558912881,0.676637683834297));
#12749=CARTESIAN_POINT('Ctrl Pts',(1.09768760301306,1.29133598921902,0.626981304916489));
#12750=CARTESIAN_POINT('Ctrl Pts',(2.16541285690349,1.31636171257899,0.6269687859393));
#12751=CARTESIAN_POINT('Ctrl Pts',(3.23292426239396,1.34330449078822,0.626960286972675));
#12752=CARTESIAN_POINT('Ctrl Pts',(4.30003720890047,1.37794098943329,0.626943772371838));
#12753=CARTESIAN_POINT('Ctrl Pts',(1.09766050997011,1.29249209748956,0.605334684996117));
#12754=CARTESIAN_POINT('Ctrl Pts',(2.16538453588699,1.31751467232976,0.605319909330946));
#12755=CARTESIAN_POINT('Ctrl Pts',(3.23289209128077,1.34445530919946,0.605309789097661));
#12756=CARTESIAN_POINT('Ctrl Pts',(4.3,1.37908752581626,0.605290299758539));
#12757=CARTESIAN_POINT('Ctrl Pts',(4.3,1.37908752581626,0.605290299758539));
#12758=CARTESIAN_POINT('Ctrl Pts',(3.23367147240841,1.34448060345116,0.605309774863278));
#12759=CARTESIAN_POINT('Ctrl Pts',(2.16694388170711,1.31755402957363,0.605319894542965));
#12760=CARTESIAN_POINT('Ctrl Pts',(1.10000000298281,1.29254692760111,0.605334652628557));
#12761=CARTESIAN_POINT('Ctrl Pts',(1.07338415738705,1.32427529283227,-8.86713457716078E-5));
#12762=CARTESIAN_POINT('Ctrl Pts',(1.08225606990759,1.31369916974318,0.201719104823349));
#12763=CARTESIAN_POINT('Ctrl Pts',(1.09112801825728,1.30312304798912,0.403526879488635));
#12764=CARTESIAN_POINT('Ctrl Pts',(1.10000000295732,1.29254692759565,0.605334652628532));
#12765=CARTESIAN_POINT('Ctrl Pts',(2.14856196511707,1.34935185539717,-5.92140853224782E-5));
#12766=CARTESIAN_POINT('Ctrl Pts',(2.15571155670469,1.33877574824882,0.201748609776328));
#12767=CARTESIAN_POINT('Ctrl Pts',(2.16286118630166,1.32819964054013,0.403556432267816));
#12768=CARTESIAN_POINT('Ctrl Pts',(2.17001085376486,1.31762353633116,0.605364253566666));
#12769=CARTESIAN_POINT('Ctrl Pts',(3.22410085073147,1.37636920007789,-3.90459518899617E-5));
#12770=CARTESIAN_POINT('Ctrl Pts',(3.22952869941811,1.36579313421484,0.201768811381317));
#12771=CARTESIAN_POINT('Ctrl Pts',(3.23495659078338,1.35521706809945,0.403576667516948));
#12772=CARTESIAN_POINT('Ctrl Pts',(3.24038452463064,1.34464100578453,0.605384522622892));
#12773=CARTESIAN_POINT('Ctrl Pts',(4.3,1.41116952203211,-1.07899800205757E-15));
#12774=CARTESIAN_POINT('Ctrl Pts',(4.3037066798556,1.40059355144758,0.201807922462832));
#12775=CARTESIAN_POINT('Ctrl Pts',(4.30741340932897,1.39001758331339,0.403615844145277));
#12776=CARTESIAN_POINT('Ctrl Pts',(4.31112018914115,1.37944161767694,0.605423765036611));
#12777=CARTESIAN_POINT('Origin',(0.9,1.39290118819044,0.));
#12778=CARTESIAN_POINT('',(0.900000001878204,-1.28788040994396,0.605337476551879));
#12779=CARTESIAN_POINT('Ctrl Pts',(0.900000001878204,-1.28788040994396,
0.605337476551879));
#12780=CARTESIAN_POINT('Ctrl Pts',(0.900000001878204,-1.29328625806092,
0.504228160928694));
#12781=CARTESIAN_POINT('Ctrl Pts',(0.899999999999999,-1.29869191435855,
0.403118132397745));
#12782=CARTESIAN_POINT('Ctrl Pts',(0.899999999999999,-1.30947917558554,
0.201339438823693));
#12783=CARTESIAN_POINT('Ctrl Pts',(0.9,-1.31486085669789,0.100669384150719));
#12784=CARTESIAN_POINT('Ctrl Pts',(0.9,-1.32024227787037,0.));
#12785=CARTESIAN_POINT('',(0.9,-1.18799600975353,0.7));
#12786=CARTESIAN_POINT('Ctrl Pts',(0.900000000000324,-1.18799600975363,
0.7));
#12787=CARTESIAN_POINT('Ctrl Pts',(0.900000000063601,-1.19590581948314,
0.699999999935493));
#12788=CARTESIAN_POINT('Ctrl Pts',(0.900000451671414,-1.20375274583281,
0.699006541951706));
#12789=CARTESIAN_POINT('Ctrl Pts',(0.900000834722547,-1.21139610511184,
0.697120084132161));
#12790=CARTESIAN_POINT('Ctrl Pts',(0.900001049758257,-1.21568690349652,
0.696061072005504));
#12791=CARTESIAN_POINT('Ctrl Pts',(0.900001241882928,-1.21991360580594,
0.694719604949841));
#12792=CARTESIAN_POINT('Ctrl Pts',(0.900001357948449,-1.22404965357203,
0.693106547509926));
#12793=CARTESIAN_POINT('Ctrl Pts',(0.900001566283472,-1.23147376710855,
0.690211145364658));
#12794=CARTESIAN_POINT('Ctrl Pts',(0.900001483882417,-1.23852542365708,
0.686475281350474));
#12795=CARTESIAN_POINT('Ctrl Pts',(0.90000115772027,-1.24505817055452,0.681980323292531));
#12796=CARTESIAN_POINT('Ctrl Pts',(0.90000097852015,-1.2486473946309,0.67951070187031));
#12797=CARTESIAN_POINT('Ctrl Pts',(0.900000731874511,-1.25207971535834,
0.676811055842604));
#12798=CARTESIAN_POINT('Ctrl Pts',(0.90000051586667,-1.25532695882913,0.673889369778116));
#12799=CARTESIAN_POINT('Ctrl Pts',(0.900000304282776,-1.25850769714062,
0.671027521295527));
#12800=CARTESIAN_POINT('Ctrl Pts',(0.900000119565725,-1.26149151526032,
0.667969976014938));
#12801=CARTESIAN_POINT('Ctrl Pts',(0.900000124706954,-1.26425564062679,
0.664728268702146));
#12802=CARTESIAN_POINT('Ctrl Pts',(0.900000134210909,-1.26936533657602,
0.658735726205464));
#12803=CARTESIAN_POINT('Ctrl Pts',(0.900000724431276,-1.2737272220214,0.652115259198653));
#12804=CARTESIAN_POINT('Ctrl Pts',(0.900000949945503,-1.27728244659665,
0.645033014705304));
#12805=CARTESIAN_POINT('Ctrl Pts',(0.900000972753073,-1.27764200720725,
0.644316745985709));
#12806=CARTESIAN_POINT('Ctrl Pts',(0.900000992743332,-1.27799327761064,
0.64359573459864));
#12807=CARTESIAN_POINT('Ctrl Pts',(0.900001009576454,-1.27833616945273,
0.642870141642621));
#12808=CARTESIAN_POINT('Ctrl Pts',(0.900001176059944,-1.28172744954266,
0.635693858502874));
#12809=CARTESIAN_POINT('Ctrl Pts',(0.900000930108723,-1.28426399347052,
0.628153947608977));
#12810=CARTESIAN_POINT('Ctrl Pts',(0.900000539908504,-1.2858931319598,0.620419547606466));
#12811=CARTESIAN_POINT('Ctrl Pts',(0.900000289636433,-1.28693805157347,
0.615458750034127));
#12812=CARTESIAN_POINT('Ctrl Pts',(0.900000000000001,-1.28760881677759,
0.610417269724172));
#12813=CARTESIAN_POINT('Ctrl Pts',(0.900000000000001,-1.28788040985668,
0.605337476551933));
#12814=CARTESIAN_POINT('',(0.9,1.18799600975353,0.7));
#12815=CARTESIAN_POINT('',(0.9,0.696450594095222,0.7));
#12816=CARTESIAN_POINT('',(0.900000001878204,1.28788040994396,0.605337476551879));
#12817=CARTESIAN_POINT('Ctrl Pts',(0.900000000000001,1.28788040985668,0.605337476551933));
#12818=CARTESIAN_POINT('Ctrl Pts',(0.900000000000001,1.28745726486871,0.613251849878237));
#12819=CARTESIAN_POINT('Ctrl Pts',(0.900000641820462,1.28606767879774,0.621075732439556));
#12820=CARTESIAN_POINT('Ctrl Pts',(0.900000906166769,1.28379497466322,0.628648019961568));
#12821=CARTESIAN_POINT('Ctrl Pts',(0.900001053446495,1.2825287445946,0.632866896498568));
#12822=CARTESIAN_POINT('Ctrl Pts',(0.900001106693909,1.28098738700664,0.637007708770872));
#12823=CARTESIAN_POINT('Ctrl Pts',(0.900001044867119,1.27917862712792,0.641040603354488));
#12824=CARTESIAN_POINT('Ctrl Pts',(0.900000933962191,1.27593407274945,0.64827481168313));
#12825=CARTESIAN_POINT('Ctrl Pts',(0.900000399592996,1.27186725264719,0.655083885116145));
#12826=CARTESIAN_POINT('Ctrl Pts',(0.900000190596867,1.2670411556595,0.661303993035384));
#12827=CARTESIAN_POINT('Ctrl Pts',(0.900000151538061,1.26613921747962,0.662466454716044));
#12828=CARTESIAN_POINT('Ctrl Pts',(0.900000126821978,1.26521063179286,0.663608275427336));
#12829=CARTESIAN_POINT('Ctrl Pts',(0.900000125264574,1.26425564063975,0.664728268702142));
#12830=CARTESIAN_POINT('Ctrl Pts',(0.90000012217056,1.26235840892454,0.66695330163032));
#12831=CARTESIAN_POINT('Ctrl Pts',(0.900000209712012,1.26035699384613,0.66909223571964));
#12832=CARTESIAN_POINT('Ctrl Pts',(0.900000331194293,1.2582587086698,0.671141334714948));
#12833=CARTESIAN_POINT('Ctrl Pts',(0.900000660246931,1.25257519443757,0.676691620936499));
#12834=CARTESIAN_POINT('Ctrl Pts',(0.900001184896248,1.24624785575673,0.681523125886843));
#12835=CARTESIAN_POINT('Ctrl Pts',(0.900001377531805,1.23944073409582,0.685581770965975));
#12836=CARTESIAN_POINT('Ctrl Pts',(0.900001499905572,1.2351164383281,0.68816006802201));
#12837=CARTESIAN_POINT('Ctrl Pts',(0.900001510509735,1.23059756718463,0.690425789971136));
#12838=CARTESIAN_POINT('Ctrl Pts',(0.900001405318139,1.22592052877826,0.692355791713551));
#12839=CARTESIAN_POINT('Ctrl Pts',(0.900001240727996,1.21860250674997,0.695375607682216));
#12840=CARTESIAN_POINT('Ctrl Pts',(0.900000792095824,1.21098234272326,0.697541065921879));
#12841=CARTESIAN_POINT('Ctrl Pts',(0.900000425437202,1.20320741268883,0.698782789564668));
#12842=CARTESIAN_POINT('Ctrl Pts',(0.900000188792485,1.19818940410026,0.699584208982791));
#12843=CARTESIAN_POINT('Ctrl Pts',(0.900000000041206,1.19310633605572,0.699999999958324));
#12844=CARTESIAN_POINT('Ctrl Pts',(0.900000000000325,1.18799600975363,0.7));
#12845=CARTESIAN_POINT('Ctrl Pts',(0.9,1.32024227787037,0.));
#12846=CARTESIAN_POINT('Ctrl Pts',(0.9,1.31486080448354,0.100670360916234));
#12847=CARTESIAN_POINT('Ctrl Pts',(0.9,1.30947907114291,0.201341392534));
#12848=CARTESIAN_POINT('Ctrl Pts',(0.9,1.2986918099064,0.403120086121531));
#12849=CARTESIAN_POINT('Ctrl Pts',(0.900000001878204,1.29328620583358,0.504229137772713));
#12850=CARTESIAN_POINT('Ctrl Pts',(0.900000001878204,1.28788040994396,0.605337476551879));
#12851=CARTESIAN_POINT('Ctrl Pts',(0.899999999999997,-1.32024227787137,
-1.86669707469278E-11));
#12852=CARTESIAN_POINT('Ctrl Pts',(0.909148787559422,-1.30966717532842,
0.201788252636133));
#12853=CARTESIAN_POINT('Ctrl Pts',(0.91829761066914,-1.29909207410335,0.403576503749508));
#12854=CARTESIAN_POINT('Ctrl Pts',(0.92744646984625,-1.28851697422138,0.605364753299354));
#12855=CARTESIAN_POINT('Ctrl Pts',(0.699273108318574,-1.31559634352334,
-5.7001548815619E-6));
#12856=CARTESIAN_POINT('Ctrl Pts',(0.708743431409066,-1.30502123870946,
0.20178254329682));
#12857=CARTESIAN_POINT('Ctrl Pts',(0.718213789763005,-1.2944461351935,0.403570785162392));
#12858=CARTESIAN_POINT('Ctrl Pts',(0.727684183892774,-1.28387103300525,
0.605359025419352));
#12859=CARTESIAN_POINT('Ctrl Pts',(0.498558799217305,-1.31100715552056,
-1.1774619888836E-5));
#12860=CARTESIAN_POINT('Ctrl Pts',(0.508350677965937,-1.30043204942944,
0.201776459055217));
#12861=CARTESIAN_POINT('Ctrl Pts',(0.518142591787393,-1.28985694462582,
0.403564691096996));
#12862=CARTESIAN_POINT('Ctrl Pts',(0.527934541191295,-1.27928184113929,
0.60535292148228));
#12863=CARTESIAN_POINT('Ctrl Pts',(0.29785707328833,-1.3064367443434,-1.84041486642056E-5));
#12864=CARTESIAN_POINT('Ctrl Pts',(0.307970527825607,-1.29586163794,0.20176981888596));
#12865=CARTESIAN_POINT('Ctrl Pts',(0.318084017341356,-1.28528653282298,
0.403558040236175));
#12866=CARTESIAN_POINT('Ctrl Pts',(0.328197542344371,-1.27471142901691,
0.605346259877786));
#12867=CARTESIAN_POINT('',(0.32957180616905,-1.2747428754212,0.605346305703265));
#12868=CARTESIAN_POINT('Ctrl Pts',(0.297857995688647,-1.306435779838,1.57426155444895E-16));
#12869=CARTESIAN_POINT('Ctrl Pts',(0.308429283449307,-1.29587142805659,
0.201782098465301));
#12870=CARTESIAN_POINT('Ctrl Pts',(0.319000553694994,-1.28530712634462,
0.403564200350135));
#12871=CARTESIAN_POINT('Ctrl Pts',(0.329571806169048,-1.2747428754212,0.605346305703266));
#12872=CARTESIAN_POINT('Ctrl Pts',(0.32957180616905,-1.2747428754212,0.605346305703265));
#12873=CARTESIAN_POINT('Ctrl Pts',(0.519721397561595,-1.27909449722757,
0.60534313598158));
#12874=CARTESIAN_POINT('Ctrl Pts',(0.709864288600121,-1.28346276435313,
0.605340219076093));
#12875=CARTESIAN_POINT('Ctrl Pts',(0.900000001879218,-1.28788040990034,
0.605337476551906));
#12876=CARTESIAN_POINT('Ctrl Pts',(0.90231940407953,-1.18804989493878,0.7));
#12877=CARTESIAN_POINT('Ctrl Pts',(0.712166351817731,-1.18363199317816,
0.7));
#12878=CARTESIAN_POINT('Ctrl Pts',(0.522011847238247,-1.17926361631973,
0.7));
#12879=CARTESIAN_POINT('Ctrl Pts',(0.331856371369203,-1.17491202960101,
0.7));
#12880=CARTESIAN_POINT('Ctrl Pts',(0.901648075315333,-1.21694488185794,
0.7));
#12881=CARTESIAN_POINT('Ctrl Pts',(0.711500071980331,-1.21252656425213,
0.69999998041973));
#12882=CARTESIAN_POINT('Ctrl Pts',(0.521348914609444,-1.20815772874132,
0.700000022626678));
#12883=CARTESIAN_POINT('Ctrl Pts',(0.331195161244126,-1.20380556524924,
0.7));
#12884=CARTESIAN_POINT('Ctrl Pts',(0.900484091294294,-1.26704448261357,
0.676664431332699));
#12885=CARTESIAN_POINT('Ctrl Pts',(0.710344780071471,-1.26262550764723,
0.676665329845182));
#12886=CARTESIAN_POINT('Ctrl Pts',(0.520199507967113,-1.25825584722226,
0.676666267597974));
#12887=CARTESIAN_POINT('Ctrl Pts',(0.3300487189482,-1.25390275839508,0.676667306001616));
#12888=CARTESIAN_POINT('Ctrl Pts',(0.90002687589075,-1.28672371253673,0.626983665342106));
#12889=CARTESIAN_POINT('Ctrl Pts',(0.709890987426059,-1.28230548388611,
0.626985988983916));
#12890=CARTESIAN_POINT('Ctrl Pts',(0.519747959090447,-1.27793661492756,
0.626988445273931));
#12891=CARTESIAN_POINT('Ctrl Pts',(0.329598318905021,-1.27358432286302,
0.626991130804315));
#12892=CARTESIAN_POINT('Ctrl Pts',(0.900000001879218,-1.28788040990034,
0.605337476551906));
#12893=CARTESIAN_POINT('Ctrl Pts',(0.709864288600121,-1.28346276435313,
0.605340219076093));
#12894=CARTESIAN_POINT('Ctrl Pts',(0.519721397561595,-1.27909449722757,
0.60534313598158));
#12895=CARTESIAN_POINT('Ctrl Pts',(0.32957180616905,-1.2747428754212,0.605346305703265));
#12896=CARTESIAN_POINT('',(0.331856371369201,-1.17491202962433,0.7));
#12897=CARTESIAN_POINT('Origin',(0.331856371539144,-1.1749120296049,0.6));
#12898=CARTESIAN_POINT('Ctrl Pts',(0.900000000000328,-1.18799600975363,
0.7));
#12899=CARTESIAN_POINT('Ctrl Pts',(0.71062007065371,-1.18359647108512,0.7));
#12900=CARTESIAN_POINT('Ctrl Pts',(0.521238702715143,-1.17924592340069,
0.7));
#12901=CARTESIAN_POINT('Ctrl Pts',(0.331856371369203,-1.17491202960101,
0.7));
#12902=CARTESIAN_POINT('Origin',(6.87409734069396,-2.22251806091942E-16,
0.7));
#12903=CARTESIAN_POINT('',(0.331856371879032,1.17491202961268,0.7));
#12904=CARTESIAN_POINT('',(0.331856371369201,-0.75,0.7));
#12905=CARTESIAN_POINT('Ctrl Pts',(0.331856371879031,1.17491202961268,0.7));
#12906=CARTESIAN_POINT('Ctrl Pts',(0.521238703055026,1.1792459234085,0.7));
#12907=CARTESIAN_POINT('Ctrl Pts',(0.710620070823648,1.18359647108907,0.7));
#12908=CARTESIAN_POINT('Ctrl Pts',(0.900000000000325,1.18799600975363,0.7));
#12909=CARTESIAN_POINT('Ctrl Pts',(0.297857073289265,1.30643674434242,-1.84041299971672E-5));
#12910=CARTESIAN_POINT('Ctrl Pts',(0.30797052782623,1.29586163793935,0.201769818898405));
#12911=CARTESIAN_POINT('Ctrl Pts',(0.318084017341667,1.28528653282265,0.403558040242397));
#12912=CARTESIAN_POINT('Ctrl Pts',(0.328197542344371,1.27471142901691,0.605346259877786));
#12913=CARTESIAN_POINT('Ctrl Pts',(0.49855879921793,1.31100715551957,-1.17746012218085E-5));
#12914=CARTESIAN_POINT('Ctrl Pts',(0.50835067796626,1.30043204942878,0.201776459067662));
#12915=CARTESIAN_POINT('Ctrl Pts',(0.518142591787414,1.28985694462549,0.403564691103219));
#12916=CARTESIAN_POINT('Ctrl Pts',(0.527934541191015,1.27928184113928,0.60535292148228));
#12917=CARTESIAN_POINT('Ctrl Pts',(0.699273108318888,1.31559634352235,-5.70013621459206E-6));
#12918=CARTESIAN_POINT('Ctrl Pts',(0.708743431409089,1.3050212387088,0.201782543309265));
#12919=CARTESIAN_POINT('Ctrl Pts',(0.718213789762737,1.29444613519316,0.403570785168614));
#12920=CARTESIAN_POINT('Ctrl Pts',(0.727684183892215,1.28387103300524,0.605359025419352));
#12921=CARTESIAN_POINT('Ctrl Pts',(0.9,1.32024227787037,-6.93889390390723E-18));
#12922=CARTESIAN_POINT('Ctrl Pts',(0.909148787559144,1.30966717532775,0.201788252648578));
#12923=CARTESIAN_POINT('Ctrl Pts',(0.918297610668582,1.29909207410301,0.403576503755731));
#12924=CARTESIAN_POINT('Ctrl Pts',(0.927446469845411,1.28851697422136,0.605364753299355));
#12925=CARTESIAN_POINT('',(0.329571806169048,1.2747428754212,0.605346305703265));
#12926=CARTESIAN_POINT('Ctrl Pts',(0.900000001879216,1.28788040990034,0.605337476551906));
#12927=CARTESIAN_POINT('Ctrl Pts',(0.709864288600119,1.28346276435313,0.605340219076093));
#12928=CARTESIAN_POINT('Ctrl Pts',(0.519721397561593,1.27909449722757,0.60534313598158));
#12929=CARTESIAN_POINT('Ctrl Pts',(0.329571806169048,1.2747428754212,0.605346305703265));
#12930=CARTESIAN_POINT('Ctrl Pts',(0.329571806169048,1.2747428754212,0.605346305703265));
#12931=CARTESIAN_POINT('Ctrl Pts',(0.319000553694994,1.28530712634462,0.403564200350134));
#12932=CARTESIAN_POINT('Ctrl Pts',(0.308429283449307,1.29587142805659,0.201782098465301));
#12933=CARTESIAN_POINT('Ctrl Pts',(0.297857995688647,1.306435779838,6.03900610074426E-17));
#12934=CARTESIAN_POINT('Ctrl Pts',(0.331856371369201,1.17491202960101,0.7));
#12935=CARTESIAN_POINT('Ctrl Pts',(0.522011847238246,1.17926361631973,0.7));
#12936=CARTESIAN_POINT('Ctrl Pts',(0.712166351817729,1.18363199317816,0.7));
#12937=CARTESIAN_POINT('Ctrl Pts',(0.902319404079528,1.18804989493878,0.7));
#12938=CARTESIAN_POINT('Ctrl Pts',(0.331195161244124,1.20380556524924,0.7));
#12939=CARTESIAN_POINT('Ctrl Pts',(0.521348914609443,1.20815772874132,0.700000022626678));
#12940=CARTESIAN_POINT('Ctrl Pts',(0.711500071980329,1.21252656425213,0.69999998041973));
#12941=CARTESIAN_POINT('Ctrl Pts',(0.901648075315331,1.21694488185794,0.7));
#12942=CARTESIAN_POINT('Ctrl Pts',(0.330048718948197,1.25390275839508,0.676667306001616));
#12943=CARTESIAN_POINT('Ctrl Pts',(0.52019950796711,1.25825584722226,0.676666267597973));
#12944=CARTESIAN_POINT('Ctrl Pts',(0.710344780071469,1.26262550764723,0.676665329845182));
#12945=CARTESIAN_POINT('Ctrl Pts',(0.900484091294292,1.26704448261357,0.676664431332698));
#12946=CARTESIAN_POINT('Ctrl Pts',(0.329598318905018,1.27358432286302,0.626991130804315));
#12947=CARTESIAN_POINT('Ctrl Pts',(0.519747959090446,1.27793661492756,0.62698844527393));
#12948=CARTESIAN_POINT('Ctrl Pts',(0.709890987426057,1.28230548388611,0.626985988983916));
#12949=CARTESIAN_POINT('Ctrl Pts',(0.900026875890748,1.28672371253673,0.626983665342106));
#12950=CARTESIAN_POINT('Ctrl Pts',(0.329571806169048,1.2747428754212,0.605346305703265));
#12951=CARTESIAN_POINT('Ctrl Pts',(0.519721397561593,1.27909449722757,0.60534313598158));
#12952=CARTESIAN_POINT('Ctrl Pts',(0.709864288600119,1.28346276435313,0.605340219076093));
#12953=CARTESIAN_POINT('Ctrl Pts',(0.900000001879216,1.28788040990034,0.605337476551906));
#12954=CARTESIAN_POINT('Origin',(0.331856371369202,1.17491202960101,0.6));
#12955=CARTESIAN_POINT('Origin',(0.331856371369202,1.17491202960101,0.6));
#12956=CARTESIAN_POINT('Origin',(0.331856371369201,1.17491202960879,0.6));
#12957=CARTESIAN_POINT('Origin',(0.331856371369202,1.17491202960101,0.6));
#12958=CARTESIAN_POINT('Origin',(12.8681436286308,1.83274446434879,0.6));
#12959=CARTESIAN_POINT('Origin',(12.8681436286308,1.83274446434879,0.6));
#12960=CARTESIAN_POINT('',(12.9680065821063,1.83274446434879,0.605233595624294));
#12961=CARTESIAN_POINT('Origin',(12.8681436286308,1.83274446434879,0.6));
#12962=CARTESIAN_POINT('Origin',(12.8681436286308,1.83274446434879,0.6));
#12963=CARTESIAN_POINT('Origin',(0.331856371369201,-1.17491202960101,0.6));
#12964=CARTESIAN_POINT('Origin',(0.331856371369201,-1.17491202960101,0.6));
#12965=CARTESIAN_POINT('Origin',(0.331856371369201,-1.17491202960101,0.6));
#12966=CARTESIAN_POINT('Origin',(0.331856371369201,-0.75,0.6));
#12967=CARTESIAN_POINT('Ctrl Pts',(0.297750759617602,-1.30654294555098,
-0.00204689530870639));
#12968=CARTESIAN_POINT('Ctrl Pts',(0.308357792853923,-1.29594287152607,
0.200417501569666));
#12969=CARTESIAN_POINT('Ctrl Pts',(0.318964808457496,-1.28534284790734,
0.40288190189057));
#12970=CARTESIAN_POINT('Ctrl Pts',(0.329571806169048,-1.2747428754212,0.605346305703266));
#12971=CARTESIAN_POINT('Ctrl Pts',(0.268364475985512,-1.30579334864515,
-0.000546070465277405));
#12972=CARTESIAN_POINT('Ctrl Pts',(0.278972236061358,-1.29519218153762,
0.201918231169276));
#12973=CARTESIAN_POINT('Ctrl Pts',(0.289579970322816,-1.28459115545203,
0.404382541571378));
#12974=CARTESIAN_POINT('Ctrl Pts',(0.300187702091134,-1.27399007937578,
0.606846849214128));
#12975=CARTESIAN_POINT('Ctrl Pts',(0.217994620733579,-1.28028753054242,
0.000758348866131992));
#12976=CARTESIAN_POINT('Ctrl Pts',(0.228604439653725,-1.26968580576698,
0.203222517770204));
#12977=CARTESIAN_POINT('Ctrl Pts',(0.239214264875756,-1.259084092946,0.405686686833815));
#12978=CARTESIAN_POINT('Ctrl Pts',(0.24982407554016,-1.24848245399652,0.608150860486448));
#12979=CARTESIAN_POINT('Ctrl Pts',(0.200221638751335,-1.22875730734246,
-0.00100806500432267));
#12980=CARTESIAN_POINT('Ctrl Pts',(0.210832346469089,-1.21815680658782,
0.201456130081263));
#12981=CARTESIAN_POINT('Ctrl Pts',(0.221443027663539,-1.20755634130466,
0.403920328365886));
#12982=CARTESIAN_POINT('Ctrl Pts',(0.232053735729819,-1.1969559383274,0.606384528499152));
#12983=CARTESIAN_POINT('Ctrl Pts',(0.200161316008396,-1.20671181983024,
-0.00215909150772397));
#12984=CARTESIAN_POINT('Ctrl Pts',(0.21077201649647,-1.19611183845239,0.200305134857769));
#12985=CARTESIAN_POINT('Ctrl Pts',(0.221382717124246,-1.18551190812967,
0.402769363888924));
#12986=CARTESIAN_POINT('Ctrl Pts',(0.231993417893744,-1.17491202960101,
0.605233595624295));
#12987=CARTESIAN_POINT('Origin',(12.8681436286308,-1.83274446434879,0.6));
#12988=CARTESIAN_POINT('',(12.9680065821063,-1.83274446434879,0.605233595624295));
#12989=CARTESIAN_POINT('Origin',(12.8681436286308,-1.83274446434879,0.6));
#12990=CARTESIAN_POINT('Origin',(12.8681436286308,-1.83274446434879,0.6));
#12991=CARTESIAN_POINT('Origin',(12.8681436286308,1.1,0.6));
#12992=CARTESIAN_POINT('',(12.9680065821063,1.1,0.605233595624295));
#12993=CARTESIAN_POINT('Ctrl Pts',(12.9998428721614,-1.86475648739599,-0.00223900654757928));
#12994=CARTESIAN_POINT('Ctrl Pts',(12.9892307746816,-1.85408610159386,0.200251876006837));
#12995=CARTESIAN_POINT('Ctrl Pts',(12.9786186779927,-1.84341542867022,0.402742743472647));
#12996=CARTESIAN_POINT('Ctrl Pts',(12.9680065821063,-1.83274446434879,0.605233595624296));
#12997=CARTESIAN_POINT('Ctrl Pts',(12.9997989521977,-1.88070362541494,-0.00140096371806573));
#12998=CARTESIAN_POINT('Ctrl Pts',(12.9891868560404,-1.87003481788623,0.2010900171988));
#12999=CARTESIAN_POINT('Ctrl Pts',(12.9785747412344,-1.85936572080465,0.403580981971657));
#13000=CARTESIAN_POINT('Ctrl Pts',(12.967962646681,-1.84869634914788,0.606071933479074));
#13001=CARTESIAN_POINT('Ctrl Pts',(12.9919061104719,-1.91252097257855,-0.00013797468654593));
#13002=CARTESIAN_POINT('Ctrl Pts',(12.9812924311808,-1.9018552985481,0.202353118580234));
#13003=CARTESIAN_POINT('Ctrl Pts',(12.970678744243,-1.89118929884075,0.404844194499128));
#13004=CARTESIAN_POINT('Ctrl Pts',(12.9600650516023,-1.88052308923615,0.607335259545336));
#13005=CARTESIAN_POINT('Ctrl Pts',(12.9539932318948,-1.95585643963679,0.000158685530800887));
#13006=CARTESIAN_POINT('Ctrl Pts',(12.9433725220626,-1.94519261899951,0.202649549046396));
#13007=CARTESIAN_POINT('Ctrl Pts',(12.9327517623504,-1.93452853669393,0.40514039680648));
#13008=CARTESIAN_POINT('Ctrl Pts',(12.9221309734579,-1.92386419524738,0.607631230057729));
#13009=CARTESIAN_POINT('Ctrl Pts',(12.9129235702791,-1.96658826742031,-0.00142816374191492));
#13010=CARTESIAN_POINT('Ctrl Pts',(12.9022969271978,-1.95592037993921,0.201062184830579));
#13011=CARTESIAN_POINT('Ctrl Pts',(12.891670251582,-1.94525202616943,0.403552507423554));
#13012=CARTESIAN_POINT('Ctrl Pts',(12.8810434760214,-1.93458357684419,0.60604282089977));
#13013=CARTESIAN_POINT('Ctrl Pts',(12.8891437477602,-1.96405813112492,-0.00280773857265357));
#13014=CARTESIAN_POINT('Ctrl Pts',(12.8785151960038,-1.95338599020215,0.199682283294402));
#13015=CARTESIAN_POINT('Ctrl Pts',(12.8678865709412,-1.94271355010484,0.402172286243574));
#13016=CARTESIAN_POINT('Ctrl Pts',(12.8572578715866,-1.93204080633595,0.604662269998931));
#13017=CARTESIAN_POINT('Ctrl Pts',(12.9997255308004,-1.86463850151065,-4.9439619065339E-17));
#13018=CARTESIAN_POINT('Ctrl Pts',(12.9891525471135,-1.85400744222428,0.201744546927532));
#13019=CARTESIAN_POINT('Ctrl Pts',(12.9785795642115,-1.84337609791338,0.403489078876654));
#13020=CARTESIAN_POINT('Ctrl Pts',(12.9680065821063,-1.83274446434879,0.605233595624296));
#13021=CARTESIAN_POINT('Ctrl Pts',(12.8891409639924,1.96405533594058,-0.00275470357795049));
#13022=CARTESIAN_POINT('Ctrl Pts',(12.8785133401458,1.95338412669368,0.199717639954231));
#13023=CARTESIAN_POINT('Ctrl Pts',(12.8678856430057,1.9427126183241,0.402189964571813));
#13024=CARTESIAN_POINT('Ctrl Pts',(12.8572578715866,1.93204080633595,0.604662269998929));
#13025=CARTESIAN_POINT('Ctrl Pts',(12.9049941793403,1.96574209420267,-0.00183498696757459));
#13026=CARTESIAN_POINT('Ctrl Pts',(12.8943678341644,1.95507368670196,0.20063757283533));
#13027=CARTESIAN_POINT('Ctrl Pts',(12.8837414238008,1.94440496992476,0.403110113573296));
#13028=CARTESIAN_POINT('Ctrl Pts',(12.8731149412098,1.93373598667478,0.605582637266155));
#13029=CARTESIAN_POINT('Ctrl Pts',(12.9374710816243,1.9613461313261,-0.000364592700753267));
#13030=CARTESIAN_POINT('Ctrl Pts',(12.9268487371951,1.95068187676899,0.202108391447626));
#13031=CARTESIAN_POINT('Ctrl Pts',(12.9162262930262,1.94001732715406,0.404581355450702));
#13032=CARTESIAN_POINT('Ctrl Pts',(12.9056038462248,1.92935253789361,0.607054307450502));
#13033=CARTESIAN_POINT('Ctrl Pts',(12.9846523118271,1.92834870343354,0.000369250346899581));
#13034=CARTESIAN_POINT('Ctrl Pts',(12.974038022963,1.91768545846127,0.202842678583437));
#13035=CARTESIAN_POINT('Ctrl Pts',(12.9634237233674,1.90702194269714,0.405316092420461));
#13036=CARTESIAN_POINT('Ctrl Pts',(12.9528094065597,1.89635817580376,0.607789492622546));
#13037=CARTESIAN_POINT('Ctrl Pts',(12.9997742127558,1.88867440031858,-0.000928907044737527));
#13038=CARTESIAN_POINT('Ctrl Pts',(12.9891630904765,1.8780073281596,0.201544447891303));
#13039=CARTESIAN_POINT('Ctrl Pts',(12.9785517991681,1.86733992038445,0.404017776344753));
#13040=CARTESIAN_POINT('Ctrl Pts',(12.9679406789684,1.85667229154743,0.606491102406462));
#13041=CARTESIAN_POINT('Ctrl Pts',(12.9998400927033,1.86475369267134,-0.00218597132744988));
#13042=CARTESIAN_POINT('Ctrl Pts',(12.9892289217097,1.85408423839396,0.200287232817622));
#13043=CARTESIAN_POINT('Ctrl Pts',(12.9786177515068,1.84341449704483,0.402760421876702));
#13044=CARTESIAN_POINT('Ctrl Pts',(12.9680065821063,1.83274446434879,0.605233595624294));
#13045=CARTESIAN_POINT('Ctrl Pts',(12.9680065821063,1.83274446434879,0.605233595624294));
#13046=CARTESIAN_POINT('Ctrl Pts',(12.9785795642115,1.84337609791338,0.403489078876654));
#13047=CARTESIAN_POINT('Ctrl Pts',(12.9891525471135,1.85400744222428,0.201744546927532));
#13048=CARTESIAN_POINT('Ctrl Pts',(12.9997255308004,1.86463850151065,1.86916454536501E-16));
#13049=CARTESIAN_POINT('Ctrl Pts',(12.6,1.80383022254432,0.7));
#13050=CARTESIAN_POINT('Ctrl Pts',(12.6893984576578,1.8133105623702,0.7));
#13051=CARTESIAN_POINT('Ctrl Pts',(12.7787800350189,1.82294762441299,0.7));
#13052=CARTESIAN_POINT('Ctrl Pts',(12.8681436286308,1.83274446434879,0.7));
#13053=CARTESIAN_POINT('Ctrl Pts',(12.5969393303222,1.83269196733649,0.7));
#13054=CARTESIAN_POINT('Ctrl Pts',(12.686303642571,1.84217134991284,0.700000098415946));
#13055=CARTESIAN_POINT('Ctrl Pts',(12.7756511334299,1.85180730951691,0.699999896874207));
#13056=CARTESIAN_POINT('Ctrl Pts',(12.8649798835675,1.86160311979107,0.7));
#13057=CARTESIAN_POINT('Ctrl Pts',(12.5916356538948,1.88270499442536,0.67643906321291));
#13058=CARTESIAN_POINT('Ctrl Pts',(12.6809412203008,1.89218243450198,0.676434576658958));
#13059=CARTESIAN_POINT('Ctrl Pts',(12.7702288461642,1.90181652272411,0.676430055978541));
#13060=CARTESIAN_POINT('Ctrl Pts',(12.8594976525144,1.91161025179704,0.676425356750174));
#13061=CARTESIAN_POINT('Ctrl Pts',(12.58957419749,1.90214427893475,0.626447702441804));
#13062=CARTESIAN_POINT('Ctrl Pts',(12.6788572782758,1.91161594713488,0.626436135819418));
#13063=CARTESIAN_POINT('Ctrl Pts',(12.7681225846323,1.92124403769089,0.626424372515079));
#13064=CARTESIAN_POINT('Ctrl Pts',(12.8573684983393,1.93103170500986,0.626412260100396));
#13065=CARTESIAN_POINT('Ctrl Pts',(12.5894662143615,1.90316254677271,0.604704117718382));
#13066=CARTESIAN_POINT('Ctrl Pts',(12.6787484942245,1.91263121188366,0.60469048808123));
#13067=CARTESIAN_POINT('Ctrl Pts',(12.7680127446979,1.92225628370762,0.604676541242762));
#13068=CARTESIAN_POINT('Ctrl Pts',(12.8572578715866,1.93204080633595,0.60466226999893));
#13069=CARTESIAN_POINT('Ctrl Pts',(0.200160815981423,1.20671231935208,-0.00216863259073552));
#13070=CARTESIAN_POINT('Ctrl Pts',(0.21077168314515,1.19611217146534,0.200298774135678));
#13071=CARTESIAN_POINT('Ctrl Pts',(0.221382550448584,1.18551207463533,0.402766183527835));
#13072=CARTESIAN_POINT('Ctrl Pts',(0.231993417893744,1.17491202960101,0.605233595624295));
#13073=CARTESIAN_POINT('Ctrl Pts',(0.200241246305444,1.23610630273461,-0.000633930584249493));
#13074=CARTESIAN_POINT('Ctrl Pts',(0.210852138766318,1.22550544237485,0.201833432539687));
#13075=CARTESIAN_POINT('Ctrl Pts',(0.221462948692539,1.21490467236247,0.404300804744641));
#13076=CARTESIAN_POINT('Ctrl Pts',(0.232073841675177,1.20430390790287,0.60676817279077));
#13077=CARTESIAN_POINT('Ctrl Pts',(0.224595236946023,1.28704077752974,0.000756396927320467));
#13078=CARTESIAN_POINT('Ctrl Pts',(0.235204871724134,1.27643877611169,0.203223757667495));
#13079=CARTESIAN_POINT('Ctrl Pts',(0.245814524913363,1.26583679641595,0.405691118453359));
#13080=CARTESIAN_POINT('Ctrl Pts',(0.256424148042823,1.25523487973404,0.608158484046399));
#13081=CARTESIAN_POINT('Ctrl Pts',(0.275710547013829,1.30598124743532,-0.000930817763883136));
#13082=CARTESIAN_POINT('Ctrl Pts',(0.286318282165364,1.29538020346814,0.201536689442792));
#13083=CARTESIAN_POINT('Ctrl Pts',(0.296926023167072,1.2847792285374,0.404004199876323));
#13084=CARTESIAN_POINT('Ctrl Pts',(0.307533728110612,1.27417827838713,0.606471713336412));
#13085=CARTESIAN_POINT('Ctrl Pts',(0.297750259763447,1.30654344507719,-0.0020564363997533));
#13086=CARTESIAN_POINT('Ctrl Pts',(0.308357459618374,1.29594320454196,0.200411140842193));
#13087=CARTESIAN_POINT('Ctrl Pts',(0.318964641840002,1.28534301441448,0.402878721526778));
#13088=CARTESIAN_POINT('Ctrl Pts',(0.329571806169048,1.2747428754212,0.605346305703265));
#13089=CARTESIAN_POINT('Origin',(13.0002740930491,2.2,-0.0104671912485888));
#13090=CARTESIAN_POINT('Origin',(0.331856371369202,1.17491202960101,0.6));
#13091=CARTESIAN_POINT('',(0.331856371879032,1.17491202961268,0.9));
#13092=CARTESIAN_POINT('',(0.0322675109428289,1.17491202960101,0.615700786872883));
#13093=CARTESIAN_POINT('Origin',(0.331856371369201,1.17491202962433,0.6));
#13094=CARTESIAN_POINT('',(0.325002675768741,1.47440456706157,0.616038917109795));
#13095=CARTESIAN_POINT('Origin',(0.331856371369202,1.17491202960101,0.6));
#13096=CARTESIAN_POINT('Origin',(0.331856371369201,1.17491202960101,0.6));
#13097=CARTESIAN_POINT('Origin',(12.8681436286308,1.83274446434879,0.6));
#13098=CARTESIAN_POINT('',(12.8681436286308,1.83274446434879,0.9));
#13099=CARTESIAN_POINT('',(12.8354863574981,2.13063349031027,0.613986809996789));
#13100=CARTESIAN_POINT('Origin',(12.8681436286308,1.83274446434879,0.6));
#13101=CARTESIAN_POINT('',(13.1677324890572,1.83274446434879,0.615700786872883));
#13102=CARTESIAN_POINT('Origin',(12.8681436286308,1.83274446434879,0.6));
#13103=CARTESIAN_POINT('Origin',(12.8681436286308,1.83274446434879,0.6));
#13104=CARTESIAN_POINT('Origin',(0.331856371369201,-1.17491202960101,0.6));
#13105=CARTESIAN_POINT('',(0.331856371369201,-1.17491202962433,0.9));
#13106=CARTESIAN_POINT('',(0.325002675768743,-1.47440456706157,0.616038917109795));
#13107=CARTESIAN_POINT('Origin',(0.331856371879032,-1.17491202961268,0.6));
#13108=CARTESIAN_POINT('',(0.0322675109428289,-1.17491202960101,0.615700786872884));
#13109=CARTESIAN_POINT('Origin',(0.331856371369201,-1.17491202960101,0.6));
#13110=CARTESIAN_POINT('Origin',(0.331856371369201,-1.17491202960101,0.6));
#13111=CARTESIAN_POINT('Origin',(0.331856371369201,-0.75,0.6));
#13112=CARTESIAN_POINT('',(0.0322675109428289,-0.75,0.615700786872883));
#13113=CARTESIAN_POINT('',(0.331856371369201,-0.75,0.9));
#13114=CARTESIAN_POINT('Ctrl Pts',(0.292429673212981,-1.5069793045954,-0.00614074949474724));
#13115=CARTESIAN_POINT('Ctrl Pts',(0.303287396789886,-1.49612100698918,
0.201252467440773));
#13116=CARTESIAN_POINT('Ctrl Pts',(0.314145064588525,-1.48526276089333,
0.408645689616972));
#13117=CARTESIAN_POINT('Ctrl Pts',(0.325002675768741,-1.47440456706157,
0.616038917109795));
#13118=CARTESIAN_POINT('Ctrl Pts',(0.204270663953122,-1.50473074636003,
-0.00163825452108868));
#13119=CARTESIAN_POINT('Ctrl Pts',(0.215130619942527,-1.49386909866124,
0.205754670272474));
#13120=CARTESIAN_POINT('Ctrl Pts',(0.225990497234893,-1.48300775583971,
0.413147615201549));
#13121=CARTESIAN_POINT('Ctrl Pts',(0.236850363534999,-1.47214617892531,
0.620540547642382));
#13122=CARTESIAN_POINT('Ctrl Pts',(0.0531014592841718,-1.42831231122466,
0.00228331220810075));
#13123=CARTESIAN_POINT('Ctrl Pts',(0.0639677431943945,-1.41744892560022,
0.209675827753147));
#13124=CARTESIAN_POINT('Ctrl Pts',(0.0748340498672138,-1.40658548887187,
0.417068339030394));
#13125=CARTESIAN_POINT('Ctrl Pts',(0.0857003072238147,-1.3957221574093,
0.624460858243749));
#13126=CARTESIAN_POINT('Ctrl Pts',(-0.000158492362241063,-1.27362248439808,
-0.0030242144278773));
#13127=CARTESIAN_POINT('Ctrl Pts',(0.0107105192099893,-1.2627628846508,
0.204368383073371));
#13128=CARTESIAN_POINT('Ctrl Pts',(0.0215794523842628,-1.25190326350425,
0.411760983371354));
#13129=CARTESIAN_POINT('Ctrl Pts',(0.0324484644510542,-1.24104375578019,
0.619153585497454));
#13130=CARTESIAN_POINT('Ctrl Pts',(-0.000339460947516079,-1.20748590713937,
-0.00647730073969574));
#13131=CARTESIAN_POINT('Ctrl Pts',(0.0105295295353408,-1.19662789414299,
0.200915392321314));
#13132=CARTESIAN_POINT('Ctrl Pts',(0.0213985201647323,-1.18576993469886,
0.408308088178364));
#13133=CARTESIAN_POINT('Ctrl Pts',(0.032267510942829,-1.17491202960101,
0.615700786872884));
#13134=CARTESIAN_POINT('Ctrl Pts',(0.292751161823634,-1.50665779898694,
4.33680868994202E-17));
#13135=CARTESIAN_POINT('Ctrl Pts',(0.30350172143464,-1.49590667092872,0.205346300540216));
#13136=CARTESIAN_POINT('Ctrl Pts',(0.314252226354851,-1.48515559337638,
0.410692606218909));
#13137=CARTESIAN_POINT('Ctrl Pts',(0.325002675768741,-1.47440456706157,
0.616038917109795));
#13138=CARTESIAN_POINT('Ctrl Pts',(0.032267510942829,-1.17491202960101,
0.615700786872884));
#13139=CARTESIAN_POINT('Ctrl Pts',(0.021511673816962,-1.18565689645617,
0.410467188483275));
#13140=CARTESIAN_POINT('Ctrl Pts',(0.0107558368367201,-1.19640181653194,
0.205233592872363));
#13141=CARTESIAN_POINT('Ctrl Pts',(-2.19605150036939E-16,-1.20714678905882,
1.11889664200504E-16));
#13142=CARTESIAN_POINT('Origin',(12.8681436286308,-1.83274446434879,0.6));
#13143=CARTESIAN_POINT('',(13.1677324890572,-1.83274446434879,0.615700786872883));
#13144=CARTESIAN_POINT('',(12.8354863574981,-2.13063349031027,0.613986809996789));
#13145=CARTESIAN_POINT('Origin',(12.8681436286308,-1.83274446434879,0.6));
#13146=CARTESIAN_POINT('',(12.8681436286308,-1.83274446434879,0.9));
#13147=CARTESIAN_POINT('Origin',(12.8681436286308,-1.83274446434879,0.6));
#13148=CARTESIAN_POINT('Origin',(12.8681436286308,-1.83274446434879,0.6));
#13149=CARTESIAN_POINT('Origin',(12.8681436286308,1.1,0.6));
#13150=CARTESIAN_POINT('',(13.1677324890572,1.1,0.615700786872883));
#13151=CARTESIAN_POINT('',(12.8681436286308,1.1,0.9));
#13152=CARTESIAN_POINT('Ctrl Pts',(12.8681436286308,-1.83274446434879,0.9));
#13153=CARTESIAN_POINT('Ctrl Pts',(11.0848390724976,-1.63724259846481,0.9));
#13154=CARTESIAN_POINT('Ctrl Pts',(6.90843812479705,-1.33014681916253,0.9));
#13155=CARTESIAN_POINT('Ctrl Pts',(2.72316671642812,-1.22963564084767,0.9));
#13156=CARTESIAN_POINT('Ctrl Pts',(0.331856371369203,-1.17491202960101,
0.9));
#13157=CARTESIAN_POINT('Ctrl Pts',(12.8586523934408,-1.91932043067563,0.9));
#13158=CARTESIAN_POINT('Ctrl Pts',(11.0774332085042,-1.7238803779394,0.89999435405169));
#13159=CARTESIAN_POINT('Ctrl Pts',(6.90489492800773,-1.41683381760594,0.900002805573959));
#13160=CARTESIAN_POINT('Ctrl Pts',(2.72111811994416,-1.31633797570969,0.90000078069347));
#13161=CARTESIAN_POINT('Ctrl Pts',(0.329872740993971,-1.26159263654569,
0.9));
#13162=CARTESIAN_POINT('Ctrl Pts',(12.8422006781022,-2.06938763738452,0.829321796184829));
#13163=CARTESIAN_POINT('Ctrl Pts',(11.0645720435655,-1.87407163985848,0.829602081442736));
#13164=CARTESIAN_POINT('Ctrl Pts',(6.89876476423634,-1.56711486110062,0.829953500700133));
#13165=CARTESIAN_POINT('Ctrl Pts',(2.71756729604702,-1.46664725828863,0.829952661937692));
#13166=CARTESIAN_POINT('Ctrl Pts',(0.326433810179884,-1.41186690836963,
0.829991693349937));
#13167=CARTESIAN_POINT('Ctrl Pts',(12.8358182377562,-2.12760618633201,0.679236780301187));
#13168=CARTESIAN_POINT('Ctrl Pts',(11.0595580661442,-1.93265366192027,0.679962478070753));
#13169=CARTESIAN_POINT('Ctrl Pts',(6.89634818471837,-1.62613750062048,0.680874066334139));
#13170=CARTESIAN_POINT('Ctrl Pts',(2.71617242066404,-1.52567909229178,0.680871998075852));
#13171=CARTESIAN_POINT('Ctrl Pts',(0.325082213976654,-1.47092890938704,
0.680973392412944));
#13172=CARTESIAN_POINT('Ctrl Pts',(12.8354863574981,-2.13063349031027,0.613986809996789));
#13173=CARTESIAN_POINT('Ctrl Pts',(11.0592740266891,-1.93586902238569,0.614841183901826));
#13174=CARTESIAN_POINT('Ctrl Pts',(6.89620783868867,-1.62958780289117,0.615922665333222));
#13175=CARTESIAN_POINT('Ctrl Pts',(2.71609101918193,-1.52912950204849,0.615919334096661));
#13176=CARTESIAN_POINT('Ctrl Pts',(0.325002675768742,-1.47440456706157,
0.616038917109795));
#13177=CARTESIAN_POINT('Ctrl Pts',(0.325002675768742,-1.47440456706157,
0.616038917109795));
#13178=CARTESIAN_POINT('Ctrl Pts',(2.71609101918193,-1.52912950204849,0.615919334096661));
#13179=CARTESIAN_POINT('Ctrl Pts',(6.89620783868867,-1.62958780289117,0.615922665333222));
#13180=CARTESIAN_POINT('Ctrl Pts',(11.0592740266891,-1.93586902238569,0.614841183901826));
#13181=CARTESIAN_POINT('Ctrl Pts',(12.8354863574981,-2.13063349031027,0.613986809996789));
#13182=CARTESIAN_POINT('Ctrl Pts',(12.8681436286308,-1.83274446434879,0.9));
#13183=CARTESIAN_POINT('Ctrl Pts',(11.0848390724976,-1.63724259846481,0.9));
#13184=CARTESIAN_POINT('Ctrl Pts',(6.90843812479705,-1.33014681916253,0.9));
#13185=CARTESIAN_POINT('Ctrl Pts',(2.72316671642812,-1.22963564084767,0.9));
#13186=CARTESIAN_POINT('Ctrl Pts',(0.331856371369203,-1.17491202960101,
0.9));
#13187=CARTESIAN_POINT('Ctrl Pts',(13.2003520234216,-1.86554403325358,-0.00671700702553119));
#13188=CARTESIAN_POINT('Ctrl Pts',(13.1894788444661,-1.85461114646479,0.200755606855839));
#13189=CARTESIAN_POINT('Ctrl Pts',(13.1786056663403,-1.84367795836273,0.40822820490283));
#13190=CARTESIAN_POINT('Ctrl Pts',(13.1677324890572,-1.83274446434879,0.615700786872884));
#13191=CARTESIAN_POINT('Ctrl Pts',(13.200220264666,-1.91338509859121,-0.00420290020003313));
#13192=CARTESIAN_POINT('Ctrl Pts',(13.1893470894366,-1.90245705934317,0.203270015787334));
#13193=CARTESIAN_POINT('Ctrl Pts',(13.1784738563058,-1.89152871992859,0.410742913234898));
#13194=CARTESIAN_POINT('Ctrl Pts',(13.1676006827814,-1.88060011874606,0.61821580043722));
#13195=CARTESIAN_POINT('Ctrl Pts',(13.1765676699515,-2.00888806967359,-0.000409897060868941));
#13196=CARTESIAN_POINT('Ctrl Pts',(13.1656896254949,-1.99796966505382,0.207063364242462));
#13197=CARTESIAN_POINT('Ctrl Pts',(13.1548115799789,-1.98705090404177,0.414536607525659));
#13198=CARTESIAN_POINT('Ctrl Pts',(13.1439334900924,-1.97613202744891,0.622009843787749));
#13199=CARTESIAN_POINT('Ctrl Pts',(13.0627995670833,-2.13884429305335,0.000475886042502645));
#13200=CARTESIAN_POINT('Ctrl Pts',(13.0518999280859,-2.12793157960824,0.207948441605934));
#13201=CARTESIAN_POINT('Ctrl Pts',(13.041000104914,-2.11701865581933,0.415420978499924));
#13202=CARTESIAN_POINT('Ctrl Pts',(13.0301002136907,-2.10610551685206,0.62289350259018));
#13203=CARTESIAN_POINT('Ctrl Pts',(12.9395973356642,-2.17103883395928,-0.00428435975826336));
#13204=CARTESIAN_POINT('Ctrl Pts',(12.9286794517625,-2.16011362679945,0.203186612960554));
#13205=CARTESIAN_POINT('Ctrl Pts',(12.9177614752639,-2.14918756369419,0.410657536673191));
#13206=CARTESIAN_POINT('Ctrl Pts',(12.9068431708026,-2.13826180183499,0.618128462699307));
#13207=CARTESIAN_POINT('Ctrl Pts',(12.8682582931239,-2.16344935299393,-0.00842301254802964));
#13208=CARTESIAN_POINT('Ctrl Pts',(12.857334548107,-2.15251107312608,0.1990469563258));
#13209=CARTESIAN_POINT('Ctrl Pts',(12.8464105706338,-2.1415724540018,0.406516897309109));
#13210=CARTESIAN_POINT('Ctrl Pts',(12.8354863574981,-2.13063349031027,0.61398680999679));
#13211=CARTESIAN_POINT('Ctrl Pts',(13.2,-1.86519007666192,-2.60208521396521E-17));
#13212=CARTESIAN_POINT('Ctrl Pts',(13.1892441622028,-1.85437516893481,0.20523361119958));
#13213=CARTESIAN_POINT('Ctrl Pts',(13.1784883252177,-1.84355996631422,0.410467206902138));
#13214=CARTESIAN_POINT('Ctrl Pts',(13.1677324890572,-1.83274446434879,0.615700786872884));
#13215=CARTESIAN_POINT('Ctrl Pts',(12.8354863574981,-2.13063349031027,0.61398680999679));
#13216=CARTESIAN_POINT('Ctrl Pts',(12.8462627343229,-2.14142441807303,0.409324567403199));
#13217=CARTESIAN_POINT('Ctrl Pts',(12.8570388818204,-2.15221501053143,0.204662297274642));
#13218=CARTESIAN_POINT('Ctrl Pts',(12.8678148030684,-2.16300527278357,2.15973072759112E-16));
#13219=CARTESIAN_POINT('Ctrl Pts',(12.868249917342,2.16344096606744,-0.0082639349430893));
#13220=CARTESIAN_POINT('Ctrl Pts',(12.8573289641336,2.15250548166836,0.19915300804817));
#13221=CARTESIAN_POINT('Ctrl Pts',(12.8464077785869,2.14156965818488,0.406569923163064));
#13222=CARTESIAN_POINT('Ctrl Pts',(12.8354863574981,2.13063349031027,0.613986809996789));
#13223=CARTESIAN_POINT('Ctrl Pts',(12.9158092820513,2.16850062662823,-0.00550483257449158));
#13224=CARTESIAN_POINT('Ctrl Pts',(12.9048922561706,2.15757374897544,0.201912774743134));
#13225=CARTESIAN_POINT('Ctrl Pts',(12.8939750281693,2.14664650750606,0.409330354360154));
#13226=CARTESIAN_POINT('Ctrl Pts',(12.8830575663678,2.13571903132675,0.616747911798467));
#13227=CARTESIAN_POINT('Ctrl Pts',(13.0132876381743,2.15534286385676,-0.00108956416640176));
#13228=CARTESIAN_POINT('Ctrl Pts',(13.002382910411,2.14442874534411,0.206329347217122));
#13229=CARTESIAN_POINT('Ctrl Pts',(12.9914779109393,2.13351435475356,0.413748232116966));
#13230=CARTESIAN_POINT('Ctrl Pts',(12.9805728576194,2.12259976690609,0.621167106093357));
#13231=CARTESIAN_POINT('Ctrl Pts',(13.1547834649542,2.05631410774027,0.001107541479323));
#13232=CARTESIAN_POINT('Ctrl Pts',(13.1439034803964,2.04540309863889,0.208527817346591));
#13233=CARTESIAN_POINT('Ctrl Pts',(13.1330234810862,2.03449182132921,0.415948079627069));
#13234=CARTESIAN_POINT('Ctrl Pts',(13.1221434051731,2.0235803832085,0.623368331037722));
#13235=CARTESIAN_POINT('Ctrl Pts',(13.2001460482598,1.93729725403583,-0.00278676680844524));
#13236=CARTESIAN_POINT('Ctrl Pts',(13.1892758011844,1.92637447722781,0.204633283810596));
#13237=CARTESIAN_POINT('Ctrl Pts',(13.1784050234814,1.91545126126866,0.412053283701094));
#13238=CARTESIAN_POINT('Ctrl Pts',(13.1675347796435,1.9045279459447,0.619473307219386));
#13239=CARTESIAN_POINT('Ctrl Pts',(13.2003436864113,1.86553565046225,-0.00655792739252892));
#13240=CARTESIAN_POINT('Ctrl Pts',(13.1894732864596,1.85460555778322,0.200861659936414));
#13241=CARTESIAN_POINT('Ctrl Pts',(13.1786028873373,1.84367516394377,0.408281231439009));
#13242=CARTESIAN_POINT('Ctrl Pts',(13.1677324890572,1.83274446434879,0.615700786872883));
#13243=CARTESIAN_POINT('Ctrl Pts',(12.8678148030684,2.16300527278357,-3.77302356024956E-17));
#13244=CARTESIAN_POINT('Ctrl Pts',(12.8570388818204,2.15221501053142,0.204662297274639));
#13245=CARTESIAN_POINT('Ctrl Pts',(12.8462627343229,2.14142441807303,0.409324567403198));
#13246=CARTESIAN_POINT('Ctrl Pts',(12.8354863574981,2.13063349031027,0.613986809996789));
#13247=CARTESIAN_POINT('Ctrl Pts',(13.1677324890572,1.83274446434879,0.615700786872883));
#13248=CARTESIAN_POINT('Ctrl Pts',(13.1784883252177,1.84355996631422,0.410467206902138));
#13249=CARTESIAN_POINT('Ctrl Pts',(13.1892441622028,1.85437516893481,0.20523361119958));
#13250=CARTESIAN_POINT('Ctrl Pts',(13.2,1.86519007666192,9.4542429440736E-17));
#13251=CARTESIAN_POINT('Ctrl Pts',(0.3318563713692,1.17491202960101,0.9));
#13252=CARTESIAN_POINT('Ctrl Pts',(2.72316671642811,1.22963564084767,0.9));
#13253=CARTESIAN_POINT('Ctrl Pts',(6.90843812479704,1.33014681916253,0.9));
#13254=CARTESIAN_POINT('Ctrl Pts',(11.0848390724976,1.63724259846481,0.9));
#13255=CARTESIAN_POINT('Ctrl Pts',(12.8681436286308,1.83274446434879,0.9));
#13256=CARTESIAN_POINT('Ctrl Pts',(0.329872740993969,1.26159263654569,0.9));
#13257=CARTESIAN_POINT('Ctrl Pts',(2.72111811994415,1.31633797570969,0.90000078069347));
#13258=CARTESIAN_POINT('Ctrl Pts',(6.90489492800774,1.41683381760594,0.90000280557396));
#13259=CARTESIAN_POINT('Ctrl Pts',(11.0774332085042,1.7238803779394,0.89999435405169));
#13260=CARTESIAN_POINT('Ctrl Pts',(12.8586523934408,1.91932043067563,0.9));
#13261=CARTESIAN_POINT('Ctrl Pts',(0.326433810179882,1.41186690836963,0.829991693349937));
#13262=CARTESIAN_POINT('Ctrl Pts',(2.71756729604703,1.46664725828863,0.829952661937692));
#13263=CARTESIAN_POINT('Ctrl Pts',(6.89876476423633,1.56711486110062,0.829953500700133));
#13264=CARTESIAN_POINT('Ctrl Pts',(11.0645720435655,1.87407163985848,0.829602081442736));
#13265=CARTESIAN_POINT('Ctrl Pts',(12.8422006781022,2.06938763738452,0.829321796184828));
#13266=CARTESIAN_POINT('Ctrl Pts',(0.325082213976652,1.47092890938703,0.680973392412944));
#13267=CARTESIAN_POINT('Ctrl Pts',(2.71617242066403,1.52567909229178,0.680871998075852));
#13268=CARTESIAN_POINT('Ctrl Pts',(6.89634818471838,1.62613750062048,0.680874066334139));
#13269=CARTESIAN_POINT('Ctrl Pts',(11.0595580661442,1.93265366192027,0.679962478070753));
#13270=CARTESIAN_POINT('Ctrl Pts',(12.8358182377562,2.12760618633201,0.679236780301187));
#13271=CARTESIAN_POINT('Ctrl Pts',(0.32500267576874,1.47440456706157,0.616038917109795));
#13272=CARTESIAN_POINT('Ctrl Pts',(2.71609101918192,1.52912950204849,0.615919334096661));
#13273=CARTESIAN_POINT('Ctrl Pts',(6.89620783868868,1.62958780289117,0.615922665333222));
#13274=CARTESIAN_POINT('Ctrl Pts',(11.0592740266891,1.93586902238569,0.614841183901826));
#13275=CARTESIAN_POINT('Ctrl Pts',(12.8354863574981,2.13063349031027,0.613986809996789));
#13276=CARTESIAN_POINT('Ctrl Pts',(12.8354863574981,2.13063349031027,0.613986809996789));
#13277=CARTESIAN_POINT('Ctrl Pts',(11.0592740266891,1.93586902238569,0.614841183901826));
#13278=CARTESIAN_POINT('Ctrl Pts',(6.89620783868868,1.62958780289117,0.615922665333222));
#13279=CARTESIAN_POINT('Ctrl Pts',(2.71609101918192,1.52912950204849,0.615919334096661));
#13280=CARTESIAN_POINT('Ctrl Pts',(0.32500267576874,1.47440456706157,0.616038917109795));
#13281=CARTESIAN_POINT('Ctrl Pts',(0.331856371879031,1.17491202961268,0.900000000000001));
#13282=CARTESIAN_POINT('Ctrl Pts',(2.72316671676804,1.22963564085583,0.9));
#13283=CARTESIAN_POINT('Ctrl Pts',(6.90843812496665,1.330146819175,0.9));
#13284=CARTESIAN_POINT('Ctrl Pts',(11.0848390724976,1.63724259846481,0.9));
#13285=CARTESIAN_POINT('Ctrl Pts',(12.8681436286308,1.83274446434879,0.9));
#13286=CARTESIAN_POINT('Ctrl Pts',(-0.00034095850043725,1.20748740317979,
-0.0065058757516861));
#13287=CARTESIAN_POINT('Ctrl Pts',(0.0105285311667133,1.19662889149835,
0.200896342313063));
#13288=CARTESIAN_POINT('Ctrl Pts',(0.0213980209804115,1.18577043337405,
0.408298563174108));
#13289=CARTESIAN_POINT('Ctrl Pts',(0.0322675109428289,1.17491202960101,
0.615700786872884));
#13290=CARTESIAN_POINT('Ctrl Pts',(-9.96670524854573E-5,1.295669506487,
-0.00190176065173685));
#13291=CARTESIAN_POINT('Ctrl Pts',(0.0107698931059531,1.28480880908357,
0.205500324005663));
#13292=CARTESIAN_POINT('Ctrl Pts',(0.0216392211477595,1.27394827585187,
0.412902429485043));
#13293=CARTESIAN_POINT('Ctrl Pts',(0.0325087822871292,1.26308766450658,
0.62030451837231));
#13294=CARTESIAN_POINT('Ctrl Pts',(0.0728623575603101,1.44853010213391,
0.00227745497540766));
#13295=CARTESIAN_POINT('Ctrl Pts',(0.0837280751164453,1.43766588856392,
0.209679530627308));
#13296=CARTESIAN_POINT('Ctrl Pts',(0.0945938325013454,1.42680163888532,
0.41708160190494));
#13297=CARTESIAN_POINT('Ctrl Pts',(0.105459512942901,1.41593747613444,0.624483681552028));
#13298=CARTESIAN_POINT('Ctrl Pts',(0.226308920038025,1.50529438233544,-0.00279245331904538));
#13299=CARTESIAN_POINT('Ctrl Pts',(0.237168779176494,1.4944331215396,0.204610074087555));
#13300=CARTESIAN_POINT('Ctrl Pts',(0.248028678199983,1.48357195724705,0.412012604182119));
#13301=CARTESIAN_POINT('Ctrl Pts',(0.258888441593434,1.47271077595937,0.619415140009235));
#13302=CARTESIAN_POINT('Ctrl Pts',(0.292428177212438,1.50698080067503,-0.00616932457891824));
#13303=CARTESIAN_POINT('Ctrl Pts',(0.303286399461314,1.49612200437087,0.201233417384176));
#13304=CARTESIAN_POINT('Ctrl Pts',(0.314144565926839,1.48526325958177,0.408636164588429));
#13305=CARTESIAN_POINT('Ctrl Pts',(0.325002675768741,1.47440456706157,0.616038917109795));
#13306=CARTESIAN_POINT('Ctrl Pts',(1.62630325872826E-19,1.20714678905882,
-9.93129189996722E-17));
#13307=CARTESIAN_POINT('Ctrl Pts',(0.0107558368367203,1.19640181653194,
0.205233592872363));
#13308=CARTESIAN_POINT('Ctrl Pts',(0.0215116738169619,1.18565689645617,
0.410467188483274));
#13309=CARTESIAN_POINT('Ctrl Pts',(0.0322675109428289,1.17491202960101,
0.615700786872884));
#13310=CARTESIAN_POINT('Ctrl Pts',(0.325002675768741,1.47440456706157,0.616038917109795));
#13311=CARTESIAN_POINT('Ctrl Pts',(0.314252226354851,1.48515559337638,0.410692606218907));
#13312=CARTESIAN_POINT('Ctrl Pts',(0.30350172143464,1.49590667092872,0.205346300540215));
#13313=CARTESIAN_POINT('Ctrl Pts',(0.292751161823635,1.50665779898694,-1.27502175484295E-16));
#13314=CARTESIAN_POINT('Ctrl Pts',(12.8678148030684,-2.16300527278356,0.));
#13315=CARTESIAN_POINT('Ctrl Pts',(12.8575947095063,-2.15224352891768,0.205346305703265));
#13316=CARTESIAN_POINT('Ctrl Pts',(12.8473746159443,-2.14148178505179,0.41069261140653));
#13317=CARTESIAN_POINT('Ctrl Pts',(12.8371545223823,-2.13072004118591,0.616038917109795));
#13318=CARTESIAN_POINT('Ctrl Pts',(8.67612692265345,-1.70561506876628,0.));
#13319=CARTESIAN_POINT('Ctrl Pts',(8.67274165808153,-1.69485332490039,0.205346305703265));
#13320=CARTESIAN_POINT('Ctrl Pts',(8.66935639350961,-1.68409158103451,0.41069261140653));
#13321=CARTESIAN_POINT('Ctrl Pts',(8.6659711289377,-1.67332983716862,0.616038917109795));
#13322=CARTESIAN_POINT('Ctrl Pts',(4.48443904223854,-1.60211086545473,0.));
#13323=CARTESIAN_POINT('Ctrl Pts',(4.48788860665674,-1.59134912158884,0.205346305703265));
#13324=CARTESIAN_POINT('Ctrl Pts',(4.49133817107494,-1.58058737772296,0.41069261140653));
#13325=CARTESIAN_POINT('Ctrl Pts',(4.49478773549313,-1.56982563385707,0.616038917109795));
#13326=CARTESIAN_POINT('Ctrl Pts',(0.292751161823634,-1.50665779898694,
0.));
#13327=CARTESIAN_POINT('Ctrl Pts',(0.303035555231945,-1.49589605512106,
0.205346305703265));
#13328=CARTESIAN_POINT('Ctrl Pts',(0.313319948640256,-1.48513431125517,
0.41069261140653));
#13329=CARTESIAN_POINT('Ctrl Pts',(0.323604342048567,-1.47437256738929,
0.616038917109795));
#13330=CARTESIAN_POINT('Origin',(0.,-1.5,0.));
#13331=CARTESIAN_POINT('Origin',(6.87409734069396,-2.22044604925031E-16,
0.9));
#13332=CARTESIAN_POINT('Ctrl Pts',(0.292751161823634,1.50665779898694,0.));
#13333=CARTESIAN_POINT('Ctrl Pts',(0.303035555231945,1.49589605512106,0.205346305703265));
#13334=CARTESIAN_POINT('Ctrl Pts',(0.313319948640256,1.48513431125517,0.41069261140653));
#13335=CARTESIAN_POINT('Ctrl Pts',(0.323604342048567,1.47437256738929,0.616038917109795));
#13336=CARTESIAN_POINT('Ctrl Pts',(4.48443904223854,1.60211086545473,0.));
#13337=CARTESIAN_POINT('Ctrl Pts',(4.48788860665674,1.59134912158884,0.205346305703265));
#13338=CARTESIAN_POINT('Ctrl Pts',(4.49133817107493,1.58058737772296,0.41069261140653));
#13339=CARTESIAN_POINT('Ctrl Pts',(4.49478773549313,1.56982563385707,0.616038917109795));
#13340=CARTESIAN_POINT('Ctrl Pts',(8.67612692265345,1.70561506876628,0.));
#13341=CARTESIAN_POINT('Ctrl Pts',(8.67274165808153,1.69485332490039,0.205346305703265));
#13342=CARTESIAN_POINT('Ctrl Pts',(8.66935639350961,1.68409158103451,0.41069261140653));
#13343=CARTESIAN_POINT('Ctrl Pts',(8.66597112893769,1.67332983716862,0.616038917109795));
#13344=CARTESIAN_POINT('Ctrl Pts',(12.8678148030684,2.16300527278356,0.));
#13345=CARTESIAN_POINT('Ctrl Pts',(12.8575947095063,2.15224352891768,0.205346305703265));
#13346=CARTESIAN_POINT('Ctrl Pts',(12.8473746159443,2.14148178505179,0.41069261140653));
#13347=CARTESIAN_POINT('Ctrl Pts',(12.8371545223823,2.13072004118591,0.616038917109795));
#13348=CARTESIAN_POINT('Origin',(13.2,2.2,0.));
#13349=CARTESIAN_POINT('',(0.,0.,0.));
#13350=CARTESIAN_POINT('Origin',(2.,0.,1.));
#13351=CARTESIAN_POINT('',(1.65,4.28626379701574E-17,1.1));
#13352=CARTESIAN_POINT('Origin',(2.,0.,1.1));
#13353=CARTESIAN_POINT('',(1.65,4.28626379701574E-17,0.9));
#13354=CARTESIAN_POINT('',(1.65,4.28626379701574E-17,1.));
#13355=CARTESIAN_POINT('Origin',(2.,0.,0.9));
#13356=CARTESIAN_POINT('Origin',(11.2,0.,1.));
#13357=CARTESIAN_POINT('',(10.85,4.28626379701574E-17,1.1));
#13358=CARTESIAN_POINT('Origin',(11.2,0.,1.1));
#13359=CARTESIAN_POINT('',(10.85,4.28626379701574E-17,0.9));
#13360=CARTESIAN_POINT('',(10.85,4.28626379701574E-17,1.));
#13361=CARTESIAN_POINT('Origin',(11.2,0.,0.9));
#13362=CARTESIAN_POINT('Origin',(9.9,1.,0.7));
#13363=CARTESIAN_POINT('',(9.65,1.,0.7));
#13364=CARTESIAN_POINT('Origin',(9.9,1.,0.7));
#13365=CARTESIAN_POINT('',(9.75,1.,0.7));
#13366=CARTESIAN_POINT('Origin',(9.9,1.,0.7));
#13367=CARTESIAN_POINT('Origin',(9.9,1.,0.7));
#13368=CARTESIAN_POINT('',(9.65,1.,0.6));
#13369=CARTESIAN_POINT('Origin',(9.9,1.,0.6));
#13370=CARTESIAN_POINT('',(9.65,1.,0.7));
#13371=CARTESIAN_POINT('Origin',(9.9,1.,0.6));
#13372=CARTESIAN_POINT('Origin',(3.3,-1.,0.7));
#13373=CARTESIAN_POINT('',(3.05,-1.,0.7));
#13374=CARTESIAN_POINT('Origin',(3.3,-1.,0.7));
#13375=CARTESIAN_POINT('',(3.15,-1.,0.7));
#13376=CARTESIAN_POINT('Origin',(3.3,-1.,0.7));
#13377=CARTESIAN_POINT('Origin',(3.3,-1.,0.7));
#13378=CARTESIAN_POINT('',(3.05,-1.,0.6));
#13379=CARTESIAN_POINT('Origin',(3.3,-1.,0.6));
#13380=CARTESIAN_POINT('',(3.05,-1.,0.7));
#13381=CARTESIAN_POINT('Origin',(3.3,-1.,0.6));
#13382=CARTESIAN_POINT('Origin',(3.3,1.,0.7));
#13383=CARTESIAN_POINT('',(3.05,1.,0.7));
#13384=CARTESIAN_POINT('Origin',(3.3,1.,0.7));
#13385=CARTESIAN_POINT('',(3.15,1.,0.7));
#13386=CARTESIAN_POINT('Origin',(3.3,1.,0.7));
#13387=CARTESIAN_POINT('Origin',(3.3,1.,0.7));
#13388=CARTESIAN_POINT('',(3.05,1.,0.6));
#13389=CARTESIAN_POINT('Origin',(3.3,1.,0.6));
#13390=CARTESIAN_POINT('',(3.05,1.,0.7));
#13391=CARTESIAN_POINT('Origin',(3.3,1.,0.6));
#13392=CARTESIAN_POINT('Origin',(9.9,-1.,0.7));
#13393=CARTESIAN_POINT('',(9.65,-1.,0.7));
#13394=CARTESIAN_POINT('Origin',(9.9,-1.,0.7));
#13395=CARTESIAN_POINT('',(9.75,-1.,0.7));
#13396=CARTESIAN_POINT('Origin',(9.9,-1.,0.7));
#13397=CARTESIAN_POINT('Origin',(9.9,-1.,0.7));
#13398=CARTESIAN_POINT('',(9.65,-1.,0.6));
#13399=CARTESIAN_POINT('Origin',(9.9,-1.,0.6));
#13400=CARTESIAN_POINT('',(9.65,-1.,0.7));
#13401=CARTESIAN_POINT('Origin',(9.9,-1.,0.6));
#13402=CARTESIAN_POINT('Origin',(9.9,1.,0.9));
#13403=CARTESIAN_POINT('',(9.75,1.,0.9));
#13404=CARTESIAN_POINT('',(9.75,1.,0.9));
#13405=CARTESIAN_POINT('Origin',(9.9,1.,0.9));
#13406=CARTESIAN_POINT('Origin',(3.3,-1.,0.9));
#13407=CARTESIAN_POINT('',(3.15,-1.,0.9));
#13408=CARTESIAN_POINT('',(3.15,-1.,0.9));
#13409=CARTESIAN_POINT('Origin',(3.3,-1.,0.9));
#13410=CARTESIAN_POINT('Origin',(3.3,1.,0.9));
#13411=CARTESIAN_POINT('',(3.15,1.,0.9));
#13412=CARTESIAN_POINT('',(3.15,1.,0.9));
#13413=CARTESIAN_POINT('Origin',(3.3,1.,0.9));
#13414=CARTESIAN_POINT('Origin',(9.9,-1.,0.9));
#13415=CARTESIAN_POINT('',(9.75,-1.,0.9));
#13416=CARTESIAN_POINT('',(9.75,-1.,0.9));
#13417=CARTESIAN_POINT('Origin',(9.9,-1.,0.9));
#13418=CARTESIAN_POINT('Ctrl Pts',(12.6883460378814,1.74710477827991,1.1));
#13419=CARTESIAN_POINT('Ctrl Pts',(12.7050904406715,1.74907248191433,1.1));
#13420=CARTESIAN_POINT('Ctrl Pts',(12.7459721545883,1.73893278412019,1.1));
#13421=CARTESIAN_POINT('Ctrl Pts',(12.7664342774515,1.70015954799943,1.1));
#13422=CARTESIAN_POINT('Ctrl Pts',(12.7664342774515,1.67768005087614,1.1));
#13423=CARTESIAN_POINT('Ctrl Pts',(12.6856343728622,1.77018000694724,1.1));
#13424=CARTESIAN_POINT('Ctrl Pts',(12.70797027111,1.77258660535003,1.09999193474305));
#13425=CARTESIAN_POINT('Ctrl Pts',(12.7620607807224,1.75878051965913,1.09998076816122));
#13426=CARTESIAN_POINT('Ctrl Pts',(12.789311301819,1.70760782583852,1.09999039212455));
#13427=CARTESIAN_POINT('Ctrl Pts',(12.7895723566779,1.67768005087614,1.1));
#13428=CARTESIAN_POINT('Ctrl Pts',(12.6809355967604,1.81016478834023,1.08112516654061));
#13429=CARTESIAN_POINT('Ctrl Pts',(12.7128933108791,1.81335099699619,1.08149246505882));
#13430=CARTESIAN_POINT('Ctrl Pts',(12.7898658458254,1.7931743676233,1.08208124913004));
#13431=CARTESIAN_POINT('Ctrl Pts',(12.8289908274994,1.72043204305838,1.08173005449524));
#13432=CARTESIAN_POINT('Ctrl Pts',(12.829672543413,1.67768005087614,1.08128963884528));
#13433=CARTESIAN_POINT('Ctrl Pts',(12.6791127113589,1.82567684354491,1.04109086533338));
#13434=CARTESIAN_POINT('Ctrl Pts',(12.7147851087716,1.82957775596959,1.04203732134162));
#13435=CARTESIAN_POINT('Ctrl Pts',(12.8014031907485,1.80754024306994,1.04357783697133));
#13436=CARTESIAN_POINT('Ctrl Pts',(12.8450621014111,1.72550665092358,1.04265503156396));
#13437=CARTESIAN_POINT('Ctrl Pts',(12.8454164251054,1.67768005087614,1.0415166534692));
#13438=CARTESIAN_POINT('Ctrl Pts',(12.6790190612712,1.82647376985122,1.02368384096639));
#13439=CARTESIAN_POINT('Ctrl Pts',(12.7148414907177,1.83063166001164,1.02479882190871));
#13440=CARTESIAN_POINT('Ctrl Pts',(12.8023492944496,1.80880756543048,1.02662811038865));
#13441=CARTESIAN_POINT('Ctrl Pts',(12.8462542441509,1.7257797841646,1.02553011374107));
#13442=CARTESIAN_POINT('Ctrl Pts',(12.8463246402318,1.67768005087614,1.02418687649944));
#13443=CARTESIAN_POINT('',(12.7664342774515,1.67768005087614,1.1));
#13444=CARTESIAN_POINT('',(12.8463246402318,1.67768005087614,1.02418687649944));
#13445=CARTESIAN_POINT('Origin',(12.7664342774515,1.67768005087614,1.02));
#13446=CARTESIAN_POINT('',(12.6790190612712,1.82647376985123,1.02368384096637));
#13447=CARTESIAN_POINT('Ctrl Pts',(12.8463246402318,1.67768005087614,1.02418687649944));
#13448=CARTESIAN_POINT('Ctrl Pts',(12.8462542441509,1.7257797841646,1.02553011374107));
#13449=CARTESIAN_POINT('Ctrl Pts',(12.8023492944496,1.80880756543048,1.02662811038865));
#13450=CARTESIAN_POINT('Ctrl Pts',(12.7148414907177,1.83063166001164,1.02479882190871));
#13451=CARTESIAN_POINT('Ctrl Pts',(12.6790190612712,1.82647376985122,1.02368384096639));
#13452=CARTESIAN_POINT('',(12.6883460378814,1.74710477827991,1.1));
#13453=CARTESIAN_POINT('Origin',(12.6883460378814,1.74710477827991,1.02));
#13454=CARTESIAN_POINT('Ctrl Pts',(12.6883460378814,1.74710477827991,1.1));
#13455=CARTESIAN_POINT('Ctrl Pts',(12.7050904406715,1.74907248191433,1.1));
#13456=CARTESIAN_POINT('Ctrl Pts',(12.7459721545883,1.73893278412019,1.1));
#13457=CARTESIAN_POINT('Ctrl Pts',(12.7664342774515,1.70015954799943,1.1));
#13458=CARTESIAN_POINT('Ctrl Pts',(12.7664342774515,1.67768005087614,1.1));
#13459=CARTESIAN_POINT('Origin',(12.7664342774515,0.926416499322631,1.02));
#13460=CARTESIAN_POINT('',(12.7664342774515,-1.67768005087614,1.1));
#13461=CARTESIAN_POINT('',(12.8463246402318,-1.67768005087614,1.02418687649944));
#13462=CARTESIAN_POINT('Origin',(12.7664342774515,-1.67768005087614,1.02));
#13463=CARTESIAN_POINT('',(12.8463246402318,0.926416499322631,1.02418687649944));
#13464=CARTESIAN_POINT('',(12.7664342774515,0.926416499322631,1.1));
#13465=CARTESIAN_POINT('Ctrl Pts',(12.7664342774515,-1.67768005087614,1.1));
#13466=CARTESIAN_POINT('Ctrl Pts',(12.7664342774515,-1.69453967371875,1.1));
#13467=CARTESIAN_POINT('Ctrl Pts',(12.7515713182712,-1.73395715258217,1.1));
#13468=CARTESIAN_POINT('Ctrl Pts',(12.7106719082684,-1.74972838312583,1.1));
#13469=CARTESIAN_POINT('Ctrl Pts',(12.6883460378814,-1.74710477827991,1.1));
#13470=CARTESIAN_POINT('Ctrl Pts',(12.7895723566779,-1.67768005087614,1.1));
#13471=CARTESIAN_POINT('Ctrl Pts',(12.7893765655337,-1.70012588209812,1.09999279409341));
#13472=CARTESIAN_POINT('Ctrl Pts',(12.7694119126837,-1.75223468493452,1.09998162170574));
#13473=CARTESIAN_POINT('Ctrl Pts',(12.7154155705261,-1.77338880481765,1.09998924632407));
#13474=CARTESIAN_POINT('Ctrl Pts',(12.6856343728622,-1.77018000694724,1.1));
#13475=CARTESIAN_POINT('Ctrl Pts',(12.829672543413,-1.67768005087614,1.08128963884528));
#13476=CARTESIAN_POINT('Ctrl Pts',(12.8291612564778,-1.70974404501309,1.08161995058275));
#13477=CARTESIAN_POINT('Ctrl Pts',(12.800330508486,-1.78383870138124,1.08209231231141));
#13478=CARTESIAN_POINT('Ctrl Pts',(12.7235458822523,-1.81441306654821,1.08161489789823));
#13479=CARTESIAN_POINT('Ctrl Pts',(12.6809355967604,-1.81016478834023,1.08112516654061));
#13480=CARTESIAN_POINT('Ctrl Pts',(12.8454164251054,-1.67768005087614,1.0415166534692));
#13481=CARTESIAN_POINT('Ctrl Pts',(12.8451506823347,-1.71355000091203,1.04237043704028));
#13482=CARTESIAN_POINT('Ctrl Pts',(12.8132193893781,-1.79702133948082,1.04360777159741));
#13483=CARTESIAN_POINT('Ctrl Pts',(12.7266759079096,-1.8308780601112,1.04235280667771));
#13484=CARTESIAN_POINT('Ctrl Pts',(12.6791127113589,-1.82567684354491,1.04109086533338));
#13485=CARTESIAN_POINT('Ctrl Pts',(12.8463246402318,-1.67768005087614,1.02418687649944));
#13486=CARTESIAN_POINT('Ctrl Pts',(12.8462718431712,-1.71375485084279,1.02519430443067));
#13487=CARTESIAN_POINT('Ctrl Pts',(12.8143456047297,-1.79814359426379,1.02666431898144));
#13488=CARTESIAN_POINT('Ctrl Pts',(12.7267823005336,-1.83201762339849,1.02517048222283));
#13489=CARTESIAN_POINT('Ctrl Pts',(12.6790190612712,-1.82647376985122,1.02368384096639));
#13490=CARTESIAN_POINT('',(12.6883460378814,-1.74710477827991,1.1));
#13491=CARTESIAN_POINT('',(12.6790190612712,-1.82647376985122,1.02368384096639));
#13492=CARTESIAN_POINT('Origin',(12.6883460378814,-1.74710477827991,1.02));
#13493=CARTESIAN_POINT('Ctrl Pts',(12.6790190612712,-1.82647376985122,1.02368384096639));
#13494=CARTESIAN_POINT('Ctrl Pts',(12.7267823005336,-1.83201762339849,1.02517048222283));
#13495=CARTESIAN_POINT('Ctrl Pts',(12.8143456047297,-1.79814359426379,1.02666431898144));
#13496=CARTESIAN_POINT('Ctrl Pts',(12.8462718431712,-1.71375485084279,1.02519430443067));
#13497=CARTESIAN_POINT('Ctrl Pts',(12.8463246402318,-1.67768005087614,1.02418687649944));
#13498=CARTESIAN_POINT('Ctrl Pts',(12.7664342774515,-1.67768005087614,1.1));
#13499=CARTESIAN_POINT('Ctrl Pts',(12.7664342774515,-1.69453967371875,1.1));
#13500=CARTESIAN_POINT('Ctrl Pts',(12.7515713182712,-1.73395715258217,1.1));
#13501=CARTESIAN_POINT('Ctrl Pts',(12.7106719082684,-1.74972838312583,1.1));
#13502=CARTESIAN_POINT('Ctrl Pts',(12.6883460378814,-1.74710477827991,1.1));
#13503=CARTESIAN_POINT('Ctrl Pts',(12.6883460378814,-1.74710477827991,1.1));
#13504=CARTESIAN_POINT('Ctrl Pts',(10.9559705848985,-1.54352621428166,1.1));
#13505=CARTESIAN_POINT('Ctrl Pts',(6.89625808461774,-1.22619725057464,1.1));
#13506=CARTESIAN_POINT('Ctrl Pts',(2.82684345252479,-1.12583341467021,1.1));
#13507=CARTESIAN_POINT('Ctrl Pts',(0.501786340825443,-1.06996858265586,
1.1));
#13508=CARTESIAN_POINT('Ctrl Pts',(12.6856343728622,-1.77018000694724,1.1));
#13509=CARTESIAN_POINT('Ctrl Pts',(10.953864459251,-1.56662322149928,1.09999817462394));
#13510=CARTESIAN_POINT('Ctrl Pts',(6.89527069668598,-1.24931220526659,1.1000008953949));
#13511=CARTESIAN_POINT('Ctrl Pts',(2.8262782431937,-1.14895306774358,1.10000025453557));
#13512=CARTESIAN_POINT('Ctrl Pts',(0.501230998995504,-1.09308153985212,
1.1));
#13513=CARTESIAN_POINT('Ctrl Pts',(12.6809355941985,-1.8101648101409,1.08112518582372));
#13514=CARTESIAN_POINT('Ctrl Pts',(10.9502073547204,-1.60665097561358,1.08120831496985));
#13515=CARTESIAN_POINT('Ctrl Pts',(6.89356335983392,-1.28937229578717,1.08131090328882));
#13516=CARTESIAN_POINT('Ctrl Pts',(2.82529878789426,-1.18902174359502,1.08130951558098));
#13517=CARTESIAN_POINT('Ctrl Pts',(0.500268515819014,-1.13313944880305,
1.0813211979534));
#13518=CARTESIAN_POINT('Ctrl Pts',(12.6791127113589,-1.82567684354491,1.04109086533338));
#13519=CARTESIAN_POINT('Ctrl Pts',(10.9487809439014,-1.62227255850559,1.04130507278566));
#13520=CARTESIAN_POINT('Ctrl Pts',(6.89288912441654,-1.30512519378816,1.04157208078929));
#13521=CARTESIAN_POINT('Ctrl Pts',(2.82491362604336,-1.2047760518259,1.04156824165415));
#13522=CARTESIAN_POINT('Ctrl Pts',(0.499889770467655,-1.14890257814483,
1.04159845594383));
#13523=CARTESIAN_POINT('Ctrl Pts',(12.6790190612712,-1.82647376985122,1.02368384096639));
#13524=CARTESIAN_POINT('Ctrl Pts',(10.9487001718726,-1.62312516854374,1.02393618996614));
#13525=CARTESIAN_POINT('Ctrl Pts',(6.89285005483575,-1.30604661809728,1.02425267661394));
#13526=CARTESIAN_POINT('Ctrl Pts',(2.82489114035621,-1.20569670918473,1.0242479474763));
#13527=CARTESIAN_POINT('Ctrl Pts',(0.499867468581681,-1.14983076778971,
1.024283610038));
#13528=CARTESIAN_POINT('',(0.501786340825443,-1.06996858265586,1.1));
#13529=CARTESIAN_POINT('',(0.499867468607324,-1.1498307677904,1.02428361003669));
#13530=CARTESIAN_POINT('Origin',(0.501786340825443,-1.06996858265586,1.02));
#13531=CARTESIAN_POINT('Ctrl Pts',(0.499867468581681,-1.14983076778971,
1.024283610038));
#13532=CARTESIAN_POINT('Ctrl Pts',(2.82489114035621,-1.20569670918473,1.0242479474763));
#13533=CARTESIAN_POINT('Ctrl Pts',(6.89285005483575,-1.30604661809728,1.02425267661394));
#13534=CARTESIAN_POINT('Ctrl Pts',(10.9487001718726,-1.62312516854374,1.02393618996614));
#13535=CARTESIAN_POINT('Ctrl Pts',(12.6790190612712,-1.82647376985122,1.02368384096639));
#13536=CARTESIAN_POINT('Ctrl Pts',(12.6883460378814,-1.74710477827991,1.1));
#13537=CARTESIAN_POINT('Ctrl Pts',(10.9559705848985,-1.54352621428166,1.1));
#13538=CARTESIAN_POINT('Ctrl Pts',(6.89625808461774,-1.22619725057464,1.1));
#13539=CARTESIAN_POINT('Ctrl Pts',(2.82684345252479,-1.12583341467021,1.1));
#13540=CARTESIAN_POINT('Ctrl Pts',(0.501786340825443,-1.06996858265586,
1.1));
#13541=CARTESIAN_POINT('Ctrl Pts',(0.501786340845132,-1.06996858265633,
1.1));
#13542=CARTESIAN_POINT('Ctrl Pts',(0.486343670353271,-1.06959753705714,
1.1));
#13543=CARTESIAN_POINT('Ctrl Pts',(0.450546621606563,-1.05636265633066,
1.1));
#13544=CARTESIAN_POINT('Ctrl Pts',(0.4335657225485,-1.02068090721437,1.1));
#13545=CARTESIAN_POINT('Ctrl Pts',(0.433565722548536,-1.00008473726807,
1.1));
#13546=CARTESIAN_POINT('Ctrl Pts',(0.501230999004731,-1.09308153985199,
1.1));
#13547=CARTESIAN_POINT('Ctrl Pts',(0.480678852604012,-1.0924131923446,1.09999359215549));
#13548=CARTESIAN_POINT('Ctrl Pts',(0.433334506735602,-1.0746197149398,1.09998454864803));
#13549=CARTESIAN_POINT('Ctrl Pts',(0.410665947227687,-1.02750530853182,
1.09999122945172));
#13550=CARTESIAN_POINT('Ctrl Pts',(0.410427643322096,-1.00008473726803,
1.1));
#13551=CARTESIAN_POINT('Ctrl Pts',(0.500268097562941,-1.13315685597024,
1.08133662520967));
#13552=CARTESIAN_POINT('Ctrl Pts',(0.470917694462572,-1.13199579109467,
1.08163072487897));
#13553=CARTESIAN_POINT('Ctrl Pts',(0.403559863183325,-1.10627672518437,
1.08206304806334));
#13554=CARTESIAN_POINT('Ctrl Pts',(0.370932263602498,-1.0392553542177,1.08170715357768));
#13555=CARTESIAN_POINT('Ctrl Pts',(0.370309959289207,-1.00008473726796,
1.08130512018932));
#13556=CARTESIAN_POINT('Ctrl Pts',(0.4998897704516,-1.14890257814396,1.04159845594539));
#13557=CARTESIAN_POINT('Ctrl Pts',(0.467042111092653,-1.1478756708603,1.04235909019736));
#13558=CARTESIAN_POINT('Ctrl Pts',(0.391210771603448,-1.11942230347982,
1.04349095641912));
#13559=CARTESIAN_POINT('Ctrl Pts',(0.354907019248534,-1.04390490695311,
1.04255582181557));
#13560=CARTESIAN_POINT('Ctrl Pts',(0.354583574894623,-1.00008473726793,
1.04151665346919));
#13561=CARTESIAN_POINT('Ctrl Pts',(0.499867468565196,-1.14983076778922,
1.02428361003984));
#13562=CARTESIAN_POINT('Ctrl Pts',(0.466823083113769,-1.14898864521809,
1.02518140264794));
#13563=CARTESIAN_POINT('Ctrl Pts',(0.390185579422885,-1.12055776822857,
1.0265258196442));
#13564=CARTESIAN_POINT('Ctrl Pts',(0.353739620824501,-1.04415516223227,
1.0254130505005));
#13565=CARTESIAN_POINT('Ctrl Pts',(0.353675359768169,-1.00008473726793,
1.02418687649943));
#13566=CARTESIAN_POINT('',(0.433565722548536,-1.00008473726807,1.1));
#13567=CARTESIAN_POINT('',(0.353675359768456,-1.00008473726778,1.0241868765049));
#13568=CARTESIAN_POINT('Origin',(0.433565722548536,-1.00008473726807,1.02));
#13569=CARTESIAN_POINT('Ctrl Pts',(0.353675359768169,-1.00008473726793,
1.02418687649943));
#13570=CARTESIAN_POINT('Ctrl Pts',(0.353739620824501,-1.04415516223227,
1.0254130505005));
#13571=CARTESIAN_POINT('Ctrl Pts',(0.390185579422885,-1.12055776822857,
1.0265258196442));
#13572=CARTESIAN_POINT('Ctrl Pts',(0.466823083113769,-1.14898864521809,
1.02518140264794));
#13573=CARTESIAN_POINT('Ctrl Pts',(0.499867468565196,-1.14983076778922,
1.02428361003984));
#13574=CARTESIAN_POINT('Ctrl Pts',(0.501786340845132,-1.06996858265633,
1.1));
#13575=CARTESIAN_POINT('Ctrl Pts',(0.486343670353271,-1.06959753705714,
1.1));
#13576=CARTESIAN_POINT('Ctrl Pts',(0.450546621606563,-1.05636265633066,
1.1));
#13577=CARTESIAN_POINT('Ctrl Pts',(0.4335657225485,-1.02068090721437,1.1));
#13578=CARTESIAN_POINT('Ctrl Pts',(0.433565722548536,-1.00008473726807,
1.1));
#13579=CARTESIAN_POINT('Origin',(0.433565722548535,-0.576416499322632,1.02));
#13580=CARTESIAN_POINT('',(0.433565722548535,1.0000847372682,1.1));
#13581=CARTESIAN_POINT('',(0.35367535976817,1.0000847372682,1.02418687649944));
#13582=CARTESIAN_POINT('Origin',(0.433565722548535,1.0000847372682,1.02));
#13583=CARTESIAN_POINT('',(0.35367535976817,-0.576416499322632,1.02418687649944));
#13584=CARTESIAN_POINT('',(0.433565722548535,-0.576416499322632,1.1));
#13585=CARTESIAN_POINT('Ctrl Pts',(0.433565722548535,1.0000847372682,1.1));
#13586=CARTESIAN_POINT('Ctrl Pts',(0.433565722548535,1.01553186472631,1.1));
#13587=CARTESIAN_POINT('Ctrl Pts',(0.445933851022605,1.05163704585376,1.1));
#13588=CARTESIAN_POINT('Ctrl Pts',(0.481196113556474,1.06947385520094,1.1));
#13589=CARTESIAN_POINT('Ctrl Pts',(0.501786340877041,1.0699685826571,1.1));
#13590=CARTESIAN_POINT('Ctrl Pts',(0.410427643322096,1.0000847372682,1.1));
#13591=CARTESIAN_POINT('Ctrl Pts',(0.410606371251307,1.0206501657139,1.09999342208879));
#13592=CARTESIAN_POINT('Ctrl Pts',(0.427269489276852,1.06840883688971,1.09998438534344));
#13593=CARTESIAN_POINT('Ctrl Pts',(0.473828137181897,1.09219040985597,1.09999145620732));
#13594=CARTESIAN_POINT('Ctrl Pts',(0.501230999047159,1.09308153985336,1.1));
#13595=CARTESIAN_POINT('Ctrl Pts',(0.370309959289211,1.0000847372682,1.08130512018932));
#13596=CARTESIAN_POINT('Ctrl Pts',(0.370776687524182,1.02946269997745,1.08160664523056));
#13597=CARTESIAN_POINT('Ctrl Pts',(0.394906927696186,1.09741901043509,1.08206104999852));
#13598=CARTESIAN_POINT('Ctrl Pts',(0.461134226826275,1.13160876948958,1.08172875810162));
#13599=CARTESIAN_POINT('Ctrl Pts',(0.500268097623607,1.13315685597264,1.08133662520906));
#13600=CARTESIAN_POINT('Ctrl Pts',(0.354583574894625,1.0000847372682,1.0415166534692));
#13601=CARTESIAN_POINT('Ctrl Pts',(0.354826158160091,1.03294986452867,1.0422960297289));
#13602=CARTESIAN_POINT('Ctrl Pts',(0.381463759848658,1.10944036955345,1.04348552759116));
#13603=CARTESIAN_POINT('Ctrl Pts',(0.456092891378057,1.14753336845448,1.04261263494683));
#13604=CARTESIAN_POINT('Ctrl Pts',(0.499889770519448,1.14890257814608,1.04159845594382));
#13605=CARTESIAN_POINT('Ctrl Pts',(0.35367535976817,1.0000847372682,1.02418687649944));
#13606=CARTESIAN_POINT('Ctrl Pts',(0.353723555560473,1.03313755598801,1.02510650700014));
#13607=CARTESIAN_POINT('Ctrl Pts',(0.380300727059747,1.11043180383933,1.02651925632578));
#13608=CARTESIAN_POINT('Ctrl Pts',(0.455808288035698,1.1487079377163,1.02548066684923));
#13609=CARTESIAN_POINT('Ctrl Pts',(0.499867468633476,1.14983076779096,1.02428361003799));
#13610=CARTESIAN_POINT('',(0.501786340877041,1.0699685826571,1.1));
#13611=CARTESIAN_POINT('',(0.499867468633699,1.14983076779054,1.0242836100458));
#13612=CARTESIAN_POINT('Origin',(0.501786340877041,1.0699685826571,1.02));
#13613=CARTESIAN_POINT('Ctrl Pts',(0.499867468633476,1.14983076779096,1.02428361003799));
#13614=CARTESIAN_POINT('Ctrl Pts',(0.455808288035698,1.1487079377163,1.02548066684923));
#13615=CARTESIAN_POINT('Ctrl Pts',(0.380300727059747,1.11043180383933,1.02651925632578));
#13616=CARTESIAN_POINT('Ctrl Pts',(0.353723555560473,1.03313755598801,1.02510650700014));
#13617=CARTESIAN_POINT('Ctrl Pts',(0.35367535976817,1.0000847372682,1.02418687649944));
#13618=CARTESIAN_POINT('Ctrl Pts',(0.433565722548535,1.0000847372682,1.1));
#13619=CARTESIAN_POINT('Ctrl Pts',(0.433565722548535,1.01553186472631,1.1));
#13620=CARTESIAN_POINT('Ctrl Pts',(0.445933851022605,1.05163704585376,1.1));
#13621=CARTESIAN_POINT('Ctrl Pts',(0.481196113556474,1.06947385520094,1.1));
#13622=CARTESIAN_POINT('Ctrl Pts',(0.501786340877041,1.0699685826571,1.1));
#13623=CARTESIAN_POINT('Ctrl Pts',(0.501786340877248,1.0699685826571,1.1));
#13624=CARTESIAN_POINT('Ctrl Pts',(2.82684356715236,1.12583341742443,1.1));
#13625=CARTESIAN_POINT('Ctrl Pts',(6.89625445951469,1.22619710828032,1.1));
#13626=CARTESIAN_POINT('Ctrl Pts',(10.9559704995293,1.54352620424957,1.1));
#13627=CARTESIAN_POINT('Ctrl Pts',(12.6883460378814,1.74710477827991,1.1));
#13628=CARTESIAN_POINT('Ctrl Pts',(0.501230999047308,1.09308153985337,1.1));
#13629=CARTESIAN_POINT('Ctrl Pts',(2.82627835782077,1.14895307049812,1.10000025453558));
#13630=CARTESIAN_POINT('Ctrl Pts',(6.89526707210341,1.24931206297629,1.10000089539479));
#13631=CARTESIAN_POINT('Ctrl Pts',(10.9538643739116,1.56662321146826,1.09999817462385));
#13632=CARTESIAN_POINT('Ctrl Pts',(12.6856343728622,1.77018000694724,1.1));
#13633=CARTESIAN_POINT('Ctrl Pts',(0.500268515870817,1.1331394488043,1.0813211979534));
#13634=CARTESIAN_POINT('Ctrl Pts',(2.82529890252049,1.18902174635009,1.08130951558041));
#13635=CARTESIAN_POINT('Ctrl Pts',(6.89355973615254,1.28937215350496,1.08131090331441));
#13636=CARTESIAN_POINT('Ctrl Pts',(10.9502072694324,1.60665096558469,1.08120831497395));
#13637=CARTESIAN_POINT('Ctrl Pts',(12.6809355941985,1.8101648101409,1.08112518582372));
#13638=CARTESIAN_POINT('Ctrl Pts',(0.499889770519458,1.14890257814608,1.04159845594383));
#13639=CARTESIAN_POINT('Ctrl Pts',(2.82491374066927,1.20477605458053,1.04156824165266));
#13640=CARTESIAN_POINT('Ctrl Pts',(6.89288550108907,1.30512505153819,1.04157208085565));
#13641=CARTESIAN_POINT('Ctrl Pts',(10.948780858633,1.62227254848209,1.04130507279621));
#13642=CARTESIAN_POINT('Ctrl Pts',(12.6791127113589,1.82567684354491,1.04109086533338));
#13643=CARTESIAN_POINT('Ctrl Pts',(0.499867468633484,1.14983076779096,1.024283610038));
#13644=CARTESIAN_POINT('Ctrl Pts',(2.82489125498211,1.205696711939,1.02424794747454));
#13645=CARTESIAN_POINT('Ctrl Pts',(6.89284643152835,1.3060464758645,1.02425267669241));
#13646=CARTESIAN_POINT('Ctrl Pts',(10.9487000866048,1.62312515852299,1.02393618997858));
#13647=CARTESIAN_POINT('Ctrl Pts',(12.6790190612712,1.82647376985123,1.02368384096639));
#13648=CARTESIAN_POINT('Ctrl Pts',(12.6790190612712,1.82647376985123,1.02368384096639));
#13649=CARTESIAN_POINT('Ctrl Pts',(10.9487000866048,1.62312515852299,1.02393618997858));
#13650=CARTESIAN_POINT('Ctrl Pts',(6.89284643152835,1.3060464758645,1.02425267669241));
#13651=CARTESIAN_POINT('Ctrl Pts',(2.82489125498211,1.205696711939,1.02424794747454));
#13652=CARTESIAN_POINT('Ctrl Pts',(0.499867468633484,1.14983076779096,1.024283610038));
#13653=CARTESIAN_POINT('Ctrl Pts',(0.501786340877248,1.0699685826571,1.1));
#13654=CARTESIAN_POINT('Ctrl Pts',(2.82684356715236,1.12583341742443,1.1));
#13655=CARTESIAN_POINT('Ctrl Pts',(6.89625445951469,1.22619710828032,1.1));
#13656=CARTESIAN_POINT('Ctrl Pts',(10.9559704995293,1.54352620424957,1.1));
#13657=CARTESIAN_POINT('Ctrl Pts',(12.6883460378814,1.74710477827991,1.1));
#13658=CARTESIAN_POINT('Origin',(0.347167001354737,-1.15283299864526,0.9));
#13659=CARTESIAN_POINT('',(0.347167001354737,1.00658943961019,0.9));
#13660=CARTESIAN_POINT('Ctrl Pts',(0.347167001354737,1.00658943961019,0.9));
#13661=CARTESIAN_POINT('Ctrl Pts',(0.349336454155793,1.00442120424608,0.941395625434512));
#13662=CARTESIAN_POINT('Ctrl Pts',(0.351505906960267,1.0022529701308,0.982791250934257));
#13663=CARTESIAN_POINT('Ctrl Pts',(0.35367535976817,1.0000847372682,1.02418687649944));
#13664=CARTESIAN_POINT('',(0.347167001354737,-1.00658943961019,0.9));
#13665=CARTESIAN_POINT('',(0.347167001354737,-1.15283299864526,0.9));
#13666=CARTESIAN_POINT('Ctrl Pts',(0.353675359768457,-1.00008473726791,
1.02418687650491));
#13667=CARTESIAN_POINT('Ctrl Pts',(0.351505906960458,-1.0022529701306,0.982791250937906));
#13668=CARTESIAN_POINT('Ctrl Pts',(0.349336454155888,-1.00442120424599,
0.941395625436337));
#13669=CARTESIAN_POINT('Ctrl Pts',(0.347167001354737,-1.00658943961019,
0.900000000000001));
#13670=CARTESIAN_POINT('Ctrl Pts',(0.346996296805428,1.00676004836741,0.896742763161407));
#13671=CARTESIAN_POINT('Ctrl Pts',(0.349222651122738,1.0045349433512,0.939224134205317));
#13672=CARTESIAN_POINT('Ctrl Pts',(0.351449005443648,1.00230983965007,0.981705505317921));
#13673=CARTESIAN_POINT('Ctrl Pts',(0.35367535976817,1.0000847372682,1.02418687649944));
#13674=CARTESIAN_POINT('Ctrl Pts',(0.347116900426942,1.05081591929015,0.899044017348554));
#13675=CARTESIAN_POINT('Ctrl Pts',(0.349343263597644,1.04859056550012,0.941525373982715));
#13676=CARTESIAN_POINT('Ctrl Pts',(0.351569598045448,1.04636522758029,0.98400673296308));
#13677=CARTESIAN_POINT('Ctrl Pts',(0.353795961241832,1.04413987589222,1.02648808970312));
#13678=CARTESIAN_POINT('Ctrl Pts',(0.383592239441417,1.12715274970112,0.901130824661994));
#13679=CARTESIAN_POINT('Ctrl Pts',(0.38581816402279,1.12492699736917,0.943612181832344));
#13680=CARTESIAN_POINT('Ctrl Pts',(0.388044096297176,1.12270123909217,0.986093538279035));
#13681=CARTESIAN_POINT('Ctrl Pts',(0.390270019973987,1.12047548800691,1.02857489555427));
#13682=CARTESIAN_POINT('Ctrl Pts',(0.460164343209507,1.15561854687756,0.898608842835867));
#13683=CARTESIAN_POINT('Ctrl Pts',(0.462389604568499,1.15339312775892,0.941090251624243));
#13684=CARTESIAN_POINT('Ctrl Pts',(0.464614871986574,1.15116771740584,0.983571660556392));
#13685=CARTESIAN_POINT('Ctrl Pts',(0.466840131020026,1.14894230022584,1.02605306955844));
#13686=CARTESIAN_POINT('Ctrl Pts',(0.493196683694039,1.15650174777388,0.896923951850831));
#13687=CARTESIAN_POINT('Ctrl Pts',(0.49542175781822,1.15427660869429,0.939405385103827));
#13688=CARTESIAN_POINT('Ctrl Pts',(0.497646830577711,1.15205147087705,0.981886818489558));
#13689=CARTESIAN_POINT('Ctrl Pts',(0.499871901968125,1.1498263343261,1.02436825200844));
#13690=CARTESIAN_POINT('',(0.493357799610229,1.15634062715414,0.9));
#13691=CARTESIAN_POINT('Ctrl Pts',(0.499867468633513,1.14983076779054,1.02428361004581));
#13692=CARTESIAN_POINT('Ctrl Pts',(0.497697580259738,1.1520007197087,0.982855739904038));
#13693=CARTESIAN_POINT('Ctrl Pts',(0.495527690583954,1.15417067283112,0.941427869888898));
#13694=CARTESIAN_POINT('Ctrl Pts',(0.493357799610229,1.15634062715414,0.9));
#13695=CARTESIAN_POINT('Ctrl Pts',(0.493357799610229,1.15634062715414,0.9));
#13696=CARTESIAN_POINT('Ctrl Pts',(0.482602647031033,1.1560824793541,0.899999999999731));
#13697=CARTESIAN_POINT('Ctrl Pts',(0.471926867235344,1.1546337250523,0.899998382330426));
#13698=CARTESIAN_POINT('Ctrl Pts',(0.461511103461674,1.15208577142905,0.899997935562642));
#13699=CARTESIAN_POINT('Ctrl Pts',(0.453002267216956,1.15000429947842,0.899997570589511));
#13700=CARTESIAN_POINT('Ctrl Pts',(0.444666263429443,1.14718801542572,0.899997957558805));
#13701=CARTESIAN_POINT('Ctrl Pts',(0.436607964282466,1.14366186386534,0.899998978246166));
#13702=CARTESIAN_POINT('Ctrl Pts',(0.426757323168539,1.13935141908028,0.900000225956719));
#13703=CARTESIAN_POINT('Ctrl Pts',(0.417425277328103,1.13402704260718,0.900002535631972));
#13704=CARTESIAN_POINT('Ctrl Pts',(0.408793513884033,1.1277570068973,0.900002417864976));
#13705=CARTESIAN_POINT('Ctrl Pts',(0.406442206080559,1.1260490379535,0.900002385785035));
#13706=CARTESIAN_POINT('Ctrl Pts',(0.404142986411405,1.12427063023042,0.900002152965402));
#13707=CARTESIAN_POINT('Ctrl Pts',(0.40189988757483,1.12242258952304,0.900001599918915));
#13708=CARTESIAN_POINT('Ctrl Pts',(0.397433290854798,1.11874265691041,0.900000498658648));
#13709=CARTESIAN_POINT('Ctrl Pts',(0.393188994678067,1.11478677136369,0.899998147353889));
#13710=CARTESIAN_POINT('Ctrl Pts',(0.389180227688998,1.11057998277971,0.899995556820878));
#13711=CARTESIAN_POINT('Ctrl Pts',(0.381747711834384,1.10278032195316,0.899990753803459));
#13712=CARTESIAN_POINT('Ctrl Pts',(0.375201641992584,1.09420365251288,0.899985427555825));
#13713=CARTESIAN_POINT('Ctrl Pts',(0.369602030462105,1.08503231460429,0.899982994308828));
#13714=CARTESIAN_POINT('Ctrl Pts',(0.365103987453251,1.07766518348509,0.899981039735804));
#13715=CARTESIAN_POINT('Ctrl Pts',(0.361217082581294,1.06991300661492,0.899980859474918));
#13716=CARTESIAN_POINT('Ctrl Pts',(0.357992910300892,1.06185737523451,0.899982473761482));
#13717=CARTESIAN_POINT('Ctrl Pts',(0.354005020049728,1.0518935857546,0.899984470428251));
#13718=CARTESIAN_POINT('Ctrl Pts',(0.351071168910505,1.04156966067519,0.899989252895565));
#13719=CARTESIAN_POINT('Ctrl Pts',(0.349267161175031,1.03104850244781,0.899993624760896));
#13720=CARTESIAN_POINT('Ctrl Pts',(0.347885225415831,1.022988911296,0.899996973769283));
#13721=CARTESIAN_POINT('Ctrl Pts',(0.347167001481006,1.014812725533,0.899999999989923));
#13722=CARTESIAN_POINT('Ctrl Pts',(0.347167001354737,1.00658943961019,0.900000000000001));
#13723=CARTESIAN_POINT('Ctrl Pts',(0.493357799610229,1.15634062715414,0.9));
#13724=CARTESIAN_POINT('Ctrl Pts',(0.495478181125715,1.15416948447463,0.941427870236244));
#13725=CARTESIAN_POINT('Ctrl Pts',(0.4975985626412,1.15199834179512,0.982855740472488));
#13726=CARTESIAN_POINT('Ctrl Pts',(0.499718944156686,1.14982719911562,1.02428361070873));
#13727=CARTESIAN_POINT('Ctrl Pts',(4.55741138981048,1.2538870134557,0.9));
#13728=CARTESIAN_POINT('Ctrl Pts',(4.55812062853622,1.25171587077619,0.941427870236244));
#13729=CARTESIAN_POINT('Ctrl Pts',(4.55882986726197,1.24954472809669,0.982855740472489));
#13730=CARTESIAN_POINT('Ctrl Pts',(4.55953910598771,1.24737358541718,1.02428361070873));
#13731=CARTESIAN_POINT('Ctrl Pts',(8.62146498001072,1.3558778793304,0.9));
#13732=CARTESIAN_POINT('Ctrl Pts',(8.62076307594673,1.35370673665089,0.941427870236244));
#13733=CARTESIAN_POINT('Ctrl Pts',(8.62006117188274,1.35153559397139,0.982855740472488));
#13734=CARTESIAN_POINT('Ctrl Pts',(8.61935926781874,1.34936445129188,1.02428361070873));
#13735=CARTESIAN_POINT('Ctrl Pts',(12.685518570211,1.83297820604925,0.9));
#13736=CARTESIAN_POINT('Ctrl Pts',(12.6834055233572,1.83080706336974,0.941427870236244));
#13737=CARTESIAN_POINT('Ctrl Pts',(12.6812924765035,1.82863592069023,0.982855740472488));
#13738=CARTESIAN_POINT('Ctrl Pts',(12.6791794296498,1.82646477801072,1.02428361070873));
#13739=CARTESIAN_POINT('',(12.685518570211,1.83297820604925,0.9));
#13740=CARTESIAN_POINT('Ctrl Pts',(12.685518570211,1.83297820604925,0.9));
#13741=CARTESIAN_POINT('Ctrl Pts',(12.6833520729681,1.83081006895277,0.941227947697879));
#13742=CARTESIAN_POINT('Ctrl Pts',(12.6811855699938,1.8286419235626,0.982455894687412));
#13743=CARTESIAN_POINT('Ctrl Pts',(12.6790190612712,1.82647376985122,1.02368384096639));
#13744=CARTESIAN_POINT('Ctrl Pts',(0.493357799610229,1.15634062715414,0.9));
#13745=CARTESIAN_POINT('Ctrl Pts',(4.55741138981048,1.2538870134557,0.9));
#13746=CARTESIAN_POINT('Ctrl Pts',(8.62146498001073,1.3558778793304,0.9));
#13747=CARTESIAN_POINT('Ctrl Pts',(12.685518570211,1.83297820604925,0.9));
#13748=CARTESIAN_POINT('Ctrl Pts',(12.6857396223418,1.83319942548878,0.895793428058847));
#13749=CARTESIAN_POINT('Ctrl Pts',(12.6834994414517,1.83095754915284,0.938423566452776));
#13750=CARTESIAN_POINT('Ctrl Pts',(12.6812592544344,1.82871566395046,0.981053704089438));
#13751=CARTESIAN_POINT('Ctrl Pts',(12.6790190612712,1.82647376985122,1.02368384096639));
#13752=CARTESIAN_POINT('Ctrl Pts',(12.7096132738247,1.83593722009608,0.897188525535458));
#13753=CARTESIAN_POINT('Ctrl Pts',(12.7073735515623,1.83369637734113,0.939818742641338));
#13754=CARTESIAN_POINT('Ctrl Pts',(12.7051338254027,1.83145551796363,0.982448958687984));
#13755=CARTESIAN_POINT('Ctrl Pts',(12.7028940916787,1.82921465970329,1.02507917444001));
#13756=CARTESIAN_POINT('Ctrl Pts',(12.7586310095219,1.82964538228831,0.8994266592275));
#13757=CARTESIAN_POINT('Ctrl Pts',(12.7563927428119,1.82740607701793,0.942057032676437));
#13758=CARTESIAN_POINT('Ctrl Pts',(12.7541544559015,1.82516675428928,0.984687404166494));
#13759=CARTESIAN_POINT('Ctrl Pts',(12.7519161806021,1.82292743696394,1.02731777659207));
#13760=CARTESIAN_POINT('Ctrl Pts',(12.8300025526753,1.78023902864912,0.90056967297836));
#13761=CARTESIAN_POINT('Ctrl Pts',(12.8277672375473,1.7780001144899,0.943200215636435));
#13762=CARTESIAN_POINT('Ctrl Pts',(12.8255319263559,1.7757611919149,0.985830758073823));
#13763=CARTESIAN_POINT('Ctrl Pts',(12.8232966088089,1.77352226682369,1.02846130007111));
#13764=CARTESIAN_POINT('Ctrl Pts',(12.8529050075203,1.72043671272769,0.898625988813541));
#13765=CARTESIAN_POINT('Ctrl Pts',(12.8506708576607,1.71819639833573,0.941256511626846));
#13766=CARTESIAN_POINT('Ctrl Pts',(12.8484366444933,1.71595605563573,0.983887029620282));
#13767=CARTESIAN_POINT('Ctrl Pts',(12.8462024947189,1.71371572743615,1.0265175517275));
#13768=CARTESIAN_POINT('Ctrl Pts',(12.853004077605,1.68438049200639,0.896735618985435));
#13769=CARTESIAN_POINT('Ctrl Pts',(12.8507699092581,1.68213930602179,0.939366090596142));
#13770=CARTESIAN_POINT('Ctrl Pts',(12.8485357409326,1.67989811224666,0.981996561798403));
#13771=CARTESIAN_POINT('Ctrl Pts',(12.8463015726285,1.67765691065502,1.02462703259085));
#13772=CARTESIAN_POINT('',(12.8528329986453,1.6842088756636,0.9));
#13773=CARTESIAN_POINT('Ctrl Pts',(12.8463246402318,1.67768005087614,1.02418687649944));
#13774=CARTESIAN_POINT('Ctrl Pts',(12.8484940930161,1.67985633316752,0.982791251385616));
#13775=CARTESIAN_POINT('Ctrl Pts',(12.8506635458206,1.68203260808875,0.941395625885387));
#13776=CARTESIAN_POINT('Ctrl Pts',(12.8528329986453,1.6842088756636,0.9));
#13777=CARTESIAN_POINT('Ctrl Pts',(12.8528329986453,1.6842088756636,0.900000000000001));
#13778=CARTESIAN_POINT('Ctrl Pts',(12.8528329990894,1.69496116035511,0.900000000031321));
#13779=CARTESIAN_POINT('Ctrl Pts',(12.8516279916809,1.7056415234076,0.899996564780585));
#13780=CARTESIAN_POINT('Ctrl Pts',(12.8493173682463,1.71608623918215,0.899994054968391));
#13781=CARTESIAN_POINT('Ctrl Pts',(12.847426586744,1.72463314262321,0.89999200119087));
#13782=CARTESIAN_POINT('Ctrl Pts',(12.8447941883809,1.73302290492875,0.899990534206534));
#13783=CARTESIAN_POINT('Ctrl Pts',(12.8414494901174,1.74115996769839,0.899990418365756));
#13784=CARTESIAN_POINT('Ctrl Pts',(12.8373567881217,1.75111679202539,0.899990276618506));
#13785=CARTESIAN_POINT('Ctrl Pts',(12.8322422209112,1.76059035368083,0.899992293328656));
#13786=CARTESIAN_POINT('Ctrl Pts',(12.8261823199623,1.76941466903515,0.899994578235276));
#13787=CARTESIAN_POINT('Ctrl Pts',(12.8228443945912,1.77427529404419,0.899995836811587));
#13788=CARTESIAN_POINT('Ctrl Pts',(12.819218773978,1.77893868154471,0.899997117508201));
#13789=CARTESIAN_POINT('Ctrl Pts',(12.8153125401773,1.78337342370743,0.899997612422461));
#13790=CARTESIAN_POINT('Ctrl Pts',(12.8134661485928,1.78546962967624,0.899997846357645));
#13791=CARTESIAN_POINT('Ctrl Pts',(12.8115570049875,1.7875146981109,0.899997899028016));
#13792=CARTESIAN_POINT('Ctrl Pts',(12.8095877759185,1.78950657520057,0.899997852068527));
#13793=CARTESIAN_POINT('Ctrl Pts',(12.802037518393,1.7971436679198,0.899997672020282));
#13794=CARTESIAN_POINT('Ctrl Pts',(12.7936869960543,1.80392089040634,0.899996345477631));
#13795=CARTESIAN_POINT('Ctrl Pts',(12.7847141304683,1.80975200096328,0.89999606036814));
#13796=CARTESIAN_POINT('Ctrl Pts',(12.7774211187199,1.81449144093269,0.899995828635385));
#13797=CARTESIAN_POINT('Ctrl Pts',(12.7697156358622,1.81860556854039,0.899996199361957));
#13798=CARTESIAN_POINT('Ctrl Pts',(12.761679297021,1.82202698480181,0.89999650903244));
#13799=CARTESIAN_POINT('Ctrl Pts',(12.7599722005109,1.82275376945776,0.899996574813315));
#13800=CARTESIAN_POINT('Ctrl Pts',(12.7582527406357,1.82344811243542,0.899996631272027));
#13801=CARTESIAN_POINT('Ctrl Pts',(12.7565217796305,1.82410952822173,0.899996662852262));
#13802=CARTESIAN_POINT('Ctrl Pts',(12.7461353325744,1.82807828316523,0.899996852346099));
#13803=CARTESIAN_POINT('Ctrl Pts',(12.7353361797362,1.83086624339127,0.899996468077086));
#13804=CARTESIAN_POINT('Ctrl Pts',(12.7243231747362,1.83245001845531,0.899997092905297));
#13805=CARTESIAN_POINT('Ctrl Pts',(12.713718016754,1.83397514123175,0.899997694594108));
#13806=CARTESIAN_POINT('Ctrl Pts',(12.702988146695,1.83437268605832,0.899999174299692));
#13807=CARTESIAN_POINT('Ctrl Pts',(12.6923097158784,1.83361665751845,0.899999788491474));
#13808=CARTESIAN_POINT('Ctrl Pts',(12.6900431251392,1.83345618381998,0.899999918859074));
#13809=CARTESIAN_POINT('Ctrl Pts',(12.6877788433122,1.83324355125563,0.900000000001074));
#13810=CARTESIAN_POINT('Ctrl Pts',(12.685518570211,1.83297820604925,0.9));
#13811=CARTESIAN_POINT('Origin',(6.88201982834292,-2.22044604925031E-16,
1.1));
#13812=CARTESIAN_POINT('Origin',(12.8528329986453,1.85283299864526,0.9));
#13813=CARTESIAN_POINT('',(12.8528329986453,-1.6842088756636,0.9));
#13814=CARTESIAN_POINT('Ctrl Pts',(12.8528329986453,-1.6842088756636,0.9));
#13815=CARTESIAN_POINT('Ctrl Pts',(12.8506635458206,-1.68203260808875,0.941395625885387));
#13816=CARTESIAN_POINT('Ctrl Pts',(12.8484940930161,-1.67985633316752,0.982791251385615));
#13817=CARTESIAN_POINT('Ctrl Pts',(12.8463246402318,-1.67768005087614,1.02418687649944));
#13818=CARTESIAN_POINT('',(12.8528329986453,1.85283299864526,0.9));
#13819=CARTESIAN_POINT('Ctrl Pts',(0.49319751180194,-1.1565009196418,0.896939762205254));
#13820=CARTESIAN_POINT('Ctrl Pts',(0.495422309889911,-1.15427605660646,
0.939415925341967));
#13821=CARTESIAN_POINT('Ctrl Pts',(0.49764710661353,-1.15205119483315,0.981892088611382));
#13822=CARTESIAN_POINT('Ctrl Pts',(0.499871901968411,-1.14982633432581,
1.02436825201392));
#13823=CARTESIAN_POINT('Ctrl Pts',(0.449154391250001,-1.15532331830903,
0.899186283506502));
#13824=CARTESIAN_POINT('Ctrl Pts',(0.451379443529967,-1.1530980743259,0.94166241338335));
#13825=CARTESIAN_POINT('Ctrl Pts',(0.453604490603533,-1.15087286444957,
0.984138545342204));
#13826=CARTESIAN_POINT('Ctrl Pts',(0.45582954070428,-1.14864762219213,1.02661467541392));
#13827=CARTESIAN_POINT('Ctrl Pts',(0.373709798968055,-1.1170292567097,0.901134386478875));
#13828=CARTESIAN_POINT('Ctrl Pts',(0.37593556973194,-1.11480381901192,0.943610469359475));
#13829=CARTESIAN_POINT('Ctrl Pts',(0.378161343437362,-1.11257837175868,
0.98608655157339));
#13830=CARTESIAN_POINT('Ctrl Pts',(0.380387113556173,-1.11035293539114,
1.02856263455032));
#13831=CARTESIAN_POINT('Ctrl Pts',(0.347087578105715,-1.039801123372,0.898484514129229));
#13832=CARTESIAN_POINT('Ctrl Pts',(0.349313658773859,-1.03757611304936,
0.940960604750146));
#13833=CARTESIAN_POINT('Ctrl Pts',(0.351539730193144,-1.03535109931323,
0.983436695671939));
#13834=CARTESIAN_POINT('Ctrl Pts',(0.353765810873703,-1.03312609123593,
1.02591278640767));
#13835=CARTESIAN_POINT('Ctrl Pts',(0.346997125389779,-1.00675922024802,
0.896758573492677));
#13836=CARTESIAN_POINT('Ctrl Pts',(0.349223203512402,-1.00453439127183,
0.939234674428006));
#13837=CARTESIAN_POINT('Ctrl Pts',(0.351449281638624,-1.0023095636104,0.98171077543201));
#13838=CARTESIAN_POINT('Ctrl Pts',(0.353675359768457,-1.00008473726791,
1.02418687650491));
#13839=CARTESIAN_POINT('',(0.493357799610228,-1.15634062715414,0.9));
#13840=CARTESIAN_POINT('Ctrl Pts',(0.347167001354737,-1.00658943961019,
0.900000000000001));
#13841=CARTESIAN_POINT('Ctrl Pts',(0.347167001425373,-1.01734828759763,
0.899999999998142));
#13842=CARTESIAN_POINT('Ctrl Pts',(0.348359077578701,-1.02805639415283,
0.899998433630397));
#13843=CARTESIAN_POINT('Ctrl Pts',(0.350656214310366,-1.0385309656087,0.899998024549738));
#13844=CARTESIAN_POINT('Ctrl Pts',(0.352533324612331,-1.04709028457193,
0.899997690268584));
#13845=CARTESIAN_POINT('Ctrl Pts',(0.355149562279486,-1.05549438497634,
0.899998101733499));
#13846=CARTESIAN_POINT('Ctrl Pts',(0.358482507184576,-1.0636377229308,0.899999127793999));
#13847=CARTESIAN_POINT('Ctrl Pts',(0.362555301547827,-1.07358872478153,
0.900000381620131));
#13848=CARTESIAN_POINT('Ctrl Pts',(0.367654000430903,-1.08304569392442,
0.900002668831236));
#13849=CARTESIAN_POINT('Ctrl Pts',(0.373714802804109,-1.09182534802447,
0.900002509451715));
#13850=CARTESIAN_POINT('Ctrl Pts',(0.375364773372187,-1.09421548879643,
0.90000246606282));
#13851=CARTESIAN_POINT('Ctrl Pts',(0.377086318771695,-1.09655531312597,
0.900002220932131));
#13852=CARTESIAN_POINT('Ctrl Pts',(0.378878733123435,-1.0988407769929,0.900001655250762));
#13853=CARTESIAN_POINT('Ctrl Pts',(0.382452759797804,-1.10339793132263,
0.900000527297116));
#13854=CARTESIAN_POINT('Ctrl Pts',(0.386308400219556,-1.10773917492176,
0.899998144709029));
#13855=CARTESIAN_POINT('Ctrl Pts',(0.390420886280218,-1.11185064093822,
0.899995523300098));
#13856=CARTESIAN_POINT('Ctrl Pts',(0.398040323803163,-1.11946818856709,
0.899990666466232));
#13857=CARTESIAN_POINT('Ctrl Pts',(0.406457812610252,-1.12621813960646,
0.899985292057237));
#13858=CARTESIAN_POINT('Ctrl Pts',(0.41549254786509,-1.13203603704298,0.899982834497606));
#13859=CARTESIAN_POINT('Ctrl Pts',(0.422749169000726,-1.13670892189372,
0.899980860606988));
#13860=CARTESIAN_POINT('Ctrl Pts',(0.430405328105449,-1.14078012415116,
0.899980677151631));
#13861=CARTESIAN_POINT('Ctrl Pts',(0.438380728308649,-1.14419607025517,
0.899982305341352));
#13862=CARTESIAN_POINT('Ctrl Pts',(0.448245442291908,-1.14842122892304,
0.899984319237269));
#13863=CARTESIAN_POINT('Ctrl Pts',(0.458495412124849,-1.1516012547891,0.899989147510445));
#13864=CARTESIAN_POINT('Ctrl Pts',(0.468969635281765,-1.1536564168707,0.899993562691215));
#13865=CARTESIAN_POINT('Ctrl Pts',(0.476989372009021,-1.15522998071208,
0.899996943236659));
#13866=CARTESIAN_POINT('Ctrl Pts',(0.485141446557615,-1.15614341614473,
0.89999999999177));
#13867=CARTESIAN_POINT('Ctrl Pts',(0.493357799610229,-1.15634062715414,
0.9));
#13868=CARTESIAN_POINT('Ctrl Pts',(0.493357799610229,-1.15634062715414,
0.9));
#13869=CARTESIAN_POINT('Ctrl Pts',(0.495527690583772,-1.1541706728313,0.941427869885423));
#13870=CARTESIAN_POINT('Ctrl Pts',(0.497697580259374,-1.15200071970906,
0.982855739897088));
#13871=CARTESIAN_POINT('Ctrl Pts',(0.499867468632967,-1.14983076779109,
1.02428361003538));
#13872=CARTESIAN_POINT('Ctrl Pts',(12.8530083952718,-1.68438482323521,0.896653232994753));
#13873=CARTESIAN_POINT('Ctrl Pts',(12.8507727877026,-1.68214219351771,0.939311166602882));
#13874=CARTESIAN_POINT('Ctrl Pts',(12.8485371801548,-1.67989955599965,0.98196909980204));
#13875=CARTESIAN_POINT('Ctrl Pts',(12.8463015726285,-1.67765691065502,1.02462703259086));
#13876=CARTESIAN_POINT('Ctrl Pts',(12.852942348552,-1.70842230260233,0.897913479482771));
#13877=CARTESIAN_POINT('Ctrl Pts',(12.8507067417858,-1.70618025058462,0.940571446443912));
#13878=CARTESIAN_POINT('Ctrl Pts',(12.8484711274102,-1.70393818829512,0.983229412467123));
#13879=CARTESIAN_POINT('Ctrl Pts',(12.8462355206888,-1.70169612184244,1.02588737868196));
#13880=CARTESIAN_POINT('Ctrl Pts',(12.8409786353997,-1.75638702494578,0.899808108153313));
#13881=CARTESIAN_POINT('Ctrl Pts',(12.838742445636,-1.75414612041198,0.942466110756886));
#13882=CARTESIAN_POINT('Ctrl Pts',(12.8365062537503,-1.75190518941781,0.985124111849326));
#13883=CARTESIAN_POINT('Ctrl Pts',(12.8342700627828,-1.74966427281549,1.02778211378599));
#13884=CARTESIAN_POINT('Ctrl Pts',(12.7836010260412,-1.82153168011476,0.900225885582409));
#13885=CARTESIAN_POINT('Ctrl Pts',(12.7813622549889,-1.8192914414386,0.942883795866658));
#13886=CARTESIAN_POINT('Ctrl Pts',(12.7791234760524,-1.81705120036295,0.985541705643422));
#13887=CARTESIAN_POINT('Ctrl Pts',(12.7768846983302,-1.81481095080325,1.02819961506361));
#13888=CARTESIAN_POINT('Ctrl Pts',(12.7215544275214,-1.83731044697508,0.89780368869924));
#13889=CARTESIAN_POINT('Ctrl Pts',(12.7193134882941,-1.83506869652207,0.940461407834127));
#13890=CARTESIAN_POINT('Ctrl Pts',(12.7170725571902,-1.83282686943458,0.983119123314088));
#13891=CARTESIAN_POINT('Ctrl Pts',(12.7148316068824,-1.83058510462933,1.02577684117682));
#13892=CARTESIAN_POINT('Ctrl Pts',(12.6857439516282,-1.83320375805174,0.895711042712126));
#13893=CARTESIAN_POINT('Ctrl Pts',(12.6835023276506,-1.83096043753957,0.938368642889274));
#13894=CARTESIAN_POINT('Ctrl Pts',(12.6812606975378,-1.82871710814956,0.981026242308181));
#13895=CARTESIAN_POINT('Ctrl Pts',(12.6790190612712,-1.82647376985122,1.02368384096639));
#13896=CARTESIAN_POINT('',(12.685518570211,-1.83297820604925,0.9));
#13897=CARTESIAN_POINT('Ctrl Pts',(12.6790190612712,-1.82647376985122,1.02368384096639));
#13898=CARTESIAN_POINT('Ctrl Pts',(12.6811855699938,-1.8286419235626,0.982455894687418));
#13899=CARTESIAN_POINT('Ctrl Pts',(12.6833520729681,-1.83081006895277,0.941227947697881));
#13900=CARTESIAN_POINT('Ctrl Pts',(12.685518570211,-1.83297820604925,0.9));
#13901=CARTESIAN_POINT('Ctrl Pts',(12.685518570211,-1.83297820604925,0.9));
#13902=CARTESIAN_POINT('Ctrl Pts',(12.6962007718831,-1.83423224573831,0.900000000027109));
#13903=CARTESIAN_POINT('Ctrl Pts',(12.7069522081469,-1.8342814865544,0.899996797888993));
#13904=CARTESIAN_POINT('Ctrl Pts',(12.7175986228217,-1.83320546389923,0.899994443686255));
#13905=CARTESIAN_POINT('Ctrl Pts',(12.7263221437181,-1.83232378622612,0.899992514685985));
#13906=CARTESIAN_POINT('Ctrl Pts',(12.7349759538105,-1.83068541925521,0.899991134073322));
#13907=CARTESIAN_POINT('Ctrl Pts',(12.7434612806603,-1.82830833949467,0.899991022249493));
#13908=CARTESIAN_POINT('Ctrl Pts',(12.7538268490808,-1.82540452879472,0.899990885646912));
#13909=CARTESIAN_POINT('Ctrl Pts',(12.7638319405548,-1.82143037312377,0.899992779825431));
#13910=CARTESIAN_POINT('Ctrl Pts',(12.7733027638617,-1.81644210162737,0.899994914291513));
#13911=CARTESIAN_POINT('Ctrl Pts',(12.7785122133597,-1.81369829070399,0.899996088359796));
#13912=CARTESIAN_POINT('Ctrl Pts',(12.7835598637901,-1.81064675361041,0.899997279965736));
#13913=CARTESIAN_POINT('Ctrl Pts',(12.7884138119185,-1.80729078554336,0.899997716205233));
#13914=CARTESIAN_POINT('Ctrl Pts',(12.7907292666901,-1.80568990476168,0.899997924302393));
#13915=CARTESIAN_POINT('Ctrl Pts',(12.7930005978609,-1.80401968744988,0.8999979548189));
#13916=CARTESIAN_POINT('Ctrl Pts',(12.7952253950699,-1.80228259226775,0.89999788947913));
#13917=CARTESIAN_POINT('Ctrl Pts',(12.8036908359575,-1.7956728767752,0.899997640858734));
#13918=CARTESIAN_POINT('Ctrl Pts',(12.8113954895597,-1.78816822909976,0.899996334032805));
#13919=CARTESIAN_POINT('Ctrl Pts',(12.818232559256,-1.77993499666286,0.899996088064289));
#13920=CARTESIAN_POINT('Ctrl Pts',(12.8237887404903,-1.77324421631459,0.899995888176659));
#13921=CARTESIAN_POINT('Ctrl Pts',(12.8287718252447,-1.76607091125846,0.899996310183797));
#13922=CARTESIAN_POINT('Ctrl Pts',(12.8331051219922,-1.75848815553817,0.899996624147351));
#13923=CARTESIAN_POINT('Ctrl Pts',(12.8340140186356,-1.75689769413573,0.899996690000312));
#13924=CARTESIAN_POINT('Ctrl Pts',(12.8348928881302,-1.75529157361675,0.899996744625968));
#13925=CARTESIAN_POINT('Ctrl Pts',(12.8357411680586,-1.75367056321155,0.89999677208873));
#13926=CARTESIAN_POINT('Ctrl Pts',(12.8409005734958,-1.74381125896804,0.89999693912265));
#13927=CARTESIAN_POINT('Ctrl Pts',(12.8449329422938,-1.7334030651393,0.899996442311536));
#13928=CARTESIAN_POINT('Ctrl Pts',(12.8477914282597,-1.72264121193733,0.899997037599541));
#13929=CARTESIAN_POINT('Ctrl Pts',(12.850541038206,-1.71228926375309,0.899997610213799));
#13930=CARTESIAN_POINT('Ctrl Pts',(12.8521849869391,-1.70168212150629,0.899999138466857));
#13931=CARTESIAN_POINT('Ctrl Pts',(12.8526768248801,-1.69099162083728,0.899999779783946));
#13932=CARTESIAN_POINT('Ctrl Pts',(12.8527806949164,-1.68873392048611,0.899999915222113));
#13933=CARTESIAN_POINT('Ctrl Pts',(12.8528329986625,-1.68647247255235,0.90000000000128));
#13934=CARTESIAN_POINT('Ctrl Pts',(12.8528329986453,-1.6842088756636,0.9));
#13935=CARTESIAN_POINT('Origin',(6.88173176806555,0.,0.9));
#13936=CARTESIAN_POINT('Ctrl Pts',(12.685518570211,-1.83297820604925,0.9));
#13937=CARTESIAN_POINT('Ctrl Pts',(8.62146498001073,-1.3558778793304,0.9));
#13938=CARTESIAN_POINT('Ctrl Pts',(4.55741138981048,-1.2538870134557,0.9));
#13939=CARTESIAN_POINT('Ctrl Pts',(0.493357799610228,-1.15634062715414,
0.9));
#13940=CARTESIAN_POINT('Ctrl Pts',(12.685518570211,-1.83297820604925,0.9));
#13941=CARTESIAN_POINT('Ctrl Pts',(12.6834055233574,-1.83080706336992,0.941427870232769));
#13942=CARTESIAN_POINT('Ctrl Pts',(12.6812924765039,-1.8286359206906,0.982855740465538));
#13943=CARTESIAN_POINT('Ctrl Pts',(12.6791794296503,-1.82646477801127,1.02428361069831));
#13944=CARTESIAN_POINT('Ctrl Pts',(8.62146498001072,-1.3558778793304,0.9));
#13945=CARTESIAN_POINT('Ctrl Pts',(8.62076307594679,-1.35370673665108,0.941427870232769));
#13946=CARTESIAN_POINT('Ctrl Pts',(8.62006117188285,-1.35153559397175,0.982855740465538));
#13947=CARTESIAN_POINT('Ctrl Pts',(8.61935926781891,-1.34936445129242,1.02428361069831));
#13948=CARTESIAN_POINT('Ctrl Pts',(4.55741138981048,-1.2538870134557,0.9));
#13949=CARTESIAN_POINT('Ctrl Pts',(4.55812062853616,-1.25171587077637,0.941427870232769));
#13950=CARTESIAN_POINT('Ctrl Pts',(4.55882986726185,-1.24954472809705,0.982855740465538));
#13951=CARTESIAN_POINT('Ctrl Pts',(4.55953910598754,-1.24737358541772,1.02428361069831));
#13952=CARTESIAN_POINT('Ctrl Pts',(0.493357799610228,-1.15634062715414,
0.9));
#13953=CARTESIAN_POINT('Ctrl Pts',(0.495478181125536,-1.15416948447481,
0.941427870232769));
#13954=CARTESIAN_POINT('Ctrl Pts',(0.497598562640844,-1.15199834179549,
0.982855740465538));
#13955=CARTESIAN_POINT('Ctrl Pts',(0.499718944156152,-1.14982719911616,
1.02428361069831));
#13956=CARTESIAN_POINT('',(0.,0.,0.));
#13957=CARTESIAN_POINT('Origin',(0.,0.,0.));
#13958=CARTESIAN_POINT('',(-0.14652705620645,9.44412402177196E-5,0.0160655045842905));
#13959=CARTESIAN_POINT('',(-0.146479946776166,0.000162062070299865,0.00893449541571059));
#13960=CARTESIAN_POINT('',(-0.14635,-1.79227059055215E-17,0.));
#13961=CARTESIAN_POINT('',(0.0634007094575209,0.131904027763685,0.));
#13962=CARTESIAN_POINT('Ctrl Pts',(-0.14652705620645,9.44412402177196E-5,
0.0160655045842905));
#13963=CARTESIAN_POINT('Ctrl Pts',(-0.146560923555419,0.00502618404349199,
0.0157963945919035));
#13964=CARTESIAN_POINT('Ctrl Pts',(-0.146333578783787,0.00995455679532004,
0.0155272845995164));
#13965=CARTESIAN_POINT('Ctrl Pts',(-0.14583475180505,0.0148550342388422,
0.0152581746071293));
#13966=CARTESIAN_POINT('Ctrl Pts',(-0.140929468554047,0.0630445487404258,
0.0126118447280274));
#13967=CARTESIAN_POINT('Ctrl Pts',(-0.10977174472993,0.108536575508351,
0.0099655148489255));
#13968=CARTESIAN_POINT('Ctrl Pts',(-0.0666135938566871,0.13056551637767,
0.00731918496982359));
#13969=CARTESIAN_POINT('Ctrl Pts',(-0.0268248419338395,0.150874636338504,
0.00487945664654906));
#13970=CARTESIAN_POINT('Ctrl Pts',(0.0231637104697219,0.151241233100125,
0.00243972832327453));
#13971=CARTESIAN_POINT('Ctrl Pts',(0.0635546915223951,0.132092229195826,
-2.16840434497101E-19));
#13972=CARTESIAN_POINT('',(-0.0634007094575146,0.131904027763688,0.));
#13973=CARTESIAN_POINT('Origin',(0.,0.,0.));
#13974=CARTESIAN_POINT('Ctrl Pts',(-0.0634007094575145,0.131904027763688,
-3.88578058618805E-16));
#13975=CARTESIAN_POINT('Ctrl Pts',(-0.107282641710421,0.110811831533068,
0.00264738937425961));
#13976=CARTESIAN_POINT('Ctrl Pts',(-0.139432201149969,0.0662847592091173,
0.00529477874851962));
#13977=CARTESIAN_POINT('Ctrl Pts',(-0.145436119191498,0.0182745223106641,
0.00794216812277962));
#13978=CARTESIAN_POINT('Ctrl Pts',(-0.146186273512714,0.0122759249909008,
0.00827294388708994));
#13979=CARTESIAN_POINT('Ctrl Pts',(-0.146528267289359,0.00622295186417552,
0.00860371965140026));
#13980=CARTESIAN_POINT('Ctrl Pts',(-0.146479946776166,0.000162062070299865,
0.00893449541571059));
#13981=CARTESIAN_POINT('Origin',(0.,0.,0.));
#13982=CARTESIAN_POINT('',(-0.146148830924315,7.59978318484386E-5,0.0660655045842905));
#13983=CARTESIAN_POINT('',(-0.146133770585873,6.2751561688711E-5,0.0589344954157103));
#13984=CARTESIAN_POINT('',(-0.14635,-1.79227059055215E-17,0.));
#13985=CARTESIAN_POINT('Ctrl Pts',(-0.146148830924315,7.59978318484386E-5,
0.0660655045842905));
#13986=CARTESIAN_POINT('Ctrl Pts',(-0.146240443598182,0.0195917497831913,
0.0650077071998482));
#13987=CARTESIAN_POINT('Ctrl Pts',(-0.142607114239671,0.0390747476468127,
0.0639499098154059));
#13988=CARTESIAN_POINT('Ctrl Pts',(-0.135087779856993,0.056920264102034,
0.0628921124309636));
#13989=CARTESIAN_POINT('Ctrl Pts',(-0.116276389754784,0.10156503643559,
0.0602457825518617));
#13990=CARTESIAN_POINT('Ctrl Pts',(-0.073143724514267,0.135961331060063,
0.0575994526727599));
#13991=CARTESIAN_POINT('Ctrl Pts',(-0.025432083612881,0.144366623974243,
0.054953122793658));
#13992=CARTESIAN_POINT('Ctrl Pts',(0.0222795572885053,0.152771916888423,
0.0523067929145561));
#13993=CARTESIAN_POINT('Ctrl Pts',(0.0745701738507606,0.135186208092309,
0.0496604630354541));
#13994=CARTESIAN_POINT('Ctrl Pts',(0.107505148494886,0.0996564726649905,
0.0470141331563522));
#13995=CARTESIAN_POINT('Ctrl Pts',(0.140440123139012,0.0641267372376721,
0.0443678032772503));
#13996=CARTESIAN_POINT('Ctrl Pts',(0.154019455865009,0.010652975179149,
0.0417214733981484));
#13997=CARTESIAN_POINT('Ctrl Pts',(0.14202839331759,-0.0362847016460775,
0.0390751435190465));
#13998=CARTESIAN_POINT('Ctrl Pts',(0.130037330770172,-0.0832223784713041,
0.0364288136399446));
#13999=CARTESIAN_POINT('Ctrl Pts',(0.0924758729493388,-0.123623970063234,
0.0337824837608427));
#14000=CARTESIAN_POINT('Ctrl Pts',(0.0465351214488668,-0.139005253038876,
0.0311361538817407));
#14001=CARTESIAN_POINT('Ctrl Pts',(0.000594369948394902,-0.154386536014517,
0.0284898240026388));
#14002=CARTESIAN_POINT('Ctrl Pts',(-0.0537256752317158,-0.144747510373871,
0.025843494123537));
#14003=CARTESIAN_POINT('Ctrl Pts',(-0.0915592764828275,-0.114484496435928,
0.0231971642444351));
#14004=CARTESIAN_POINT('Ctrl Pts',(-0.125545511528741,-0.0872989822136326,
0.0208199443577202));
#14005=CARTESIAN_POINT('Ctrl Pts',(-0.146227884351973,-0.0434707826450544,
0.0184427244710054));
#14006=CARTESIAN_POINT('Ctrl Pts',(-0.14652705620645,9.44412402177196E-5,
0.0160655045842905));
#14007=CARTESIAN_POINT('Ctrl Pts',(-0.146479946776166,0.000162062070299865,
0.00893449541571059));
#14008=CARTESIAN_POINT('Ctrl Pts',(-0.146141530330399,-0.0422858476614564,
0.0112511090256603));
#14009=CARTESIAN_POINT('Ctrl Pts',(-0.126658161292025,-0.0851220706608281,
0.0135677226356099));
#14010=CARTESIAN_POINT('Ctrl Pts',(-0.0941604943243988,-0.112386678841155,
0.0158843362455596));
#14011=CARTESIAN_POINT('Ctrl Pts',(-0.0570226747722624,-0.143544241621566,
0.0185317256198196));
#14012=CARTESIAN_POINT('Ctrl Pts',(-0.00288875902448078,-0.154365965709432,
0.0211791149940796));
#14013=CARTESIAN_POINT('Ctrl Pts',(0.0434083729543798,-0.140002007265973,
0.0238265043683396));
#14014=CARTESIAN_POINT('Ctrl Pts',(0.0897055049332404,-0.125638048822514,
0.0264738937425996));
#14015=CARTESIAN_POINT('Ctrl Pts',(0.12816585314318,-0.0860884078477292,
0.0291212831168596));
#14016=CARTESIAN_POINT('Ctrl Pts',(0.141191617966992,-0.0394144013492358,
0.0317686724911196));
#14017=CARTESIAN_POINT('Ctrl Pts',(0.154217382790803,0.00725960514925768,
0.0344160618653796));
#14018=CARTESIAN_POINT('Ctrl Pts',(0.141808564228487,0.0610579771714599,
0.0370634512396396));
#14019=CARTESIAN_POINT('Ctrl Pts',(0.109639063769471,0.0973098477439542,
0.0397108406138996));
#14020=CARTESIAN_POINT('Ctrl Pts',(0.0774695633104545,0.133561718316448,
0.0423582299881596));
#14021=CARTESIAN_POINT('Ctrl Pts',(0.0255393809547383,0.152267087439235,
0.0450056193624196));
#14022=CARTESIAN_POINT('Ctrl Pts',(-0.0223595433272462,0.144872892294413,
0.0476530087366796));
#14023=CARTESIAN_POINT('Ctrl Pts',(-0.070258467609231,0.137478697149591,
0.0503003981109396));
#14024=CARTESIAN_POINT('Ctrl Pts',(-0.114126133817484,0.10398493773716,
0.0529477874851996));
#14025=CARTESIAN_POINT('Ctrl Pts',(-0.133871661545403,0.059725601630819,
0.0555951768594596));
#14026=CARTESIAN_POINT('Ctrl Pts',(-0.142173753131161,0.0411165744656389,
0.0567082830448765));
#14027=CARTESIAN_POINT('Ctrl Pts',(-0.146211489678532,0.0206043892842972,
0.0578213892302934));
#14028=CARTESIAN_POINT('Ctrl Pts',(-0.146133770585873,6.2751561688711E-5,
0.0589344954157103));
#14029=CARTESIAN_POINT('Origin',(0.,0.,0.));
#14030=CARTESIAN_POINT('',(-0.146252097264499,-0.000124487410312429,0.116065504584291));
#14031=CARTESIAN_POINT('',(-0.146276374479508,-0.000129480650117819,0.10893449541571));
#14032=CARTESIAN_POINT('',(-0.14635,-1.79227059055215E-17,0.));
#14033=CARTESIAN_POINT('Ctrl Pts',(-0.146252097264499,-0.000124487410312429,
0.116065504584291));
#14034=CARTESIAN_POINT('Ctrl Pts',(-0.145977101830714,0.0338815411246725,
0.114219019807793));
#14035=CARTESIAN_POINT('Ctrl Pts',(-0.134160879762789,0.0680598926014691,
0.112372535031295));
#14036=CARTESIAN_POINT('Ctrl Pts',(-0.112484833627769,0.0939988017516943,
0.110526050254798));
#14037=CARTESIAN_POINT('Ctrl Pts',(-0.0814193359437304,0.131173714423195,
0.107879720375696));
#14038=CARTESIAN_POINT('Ctrl Pts',(-0.0301019434218634,0.151424966146533,
0.105233390496594));
#14039=CARTESIAN_POINT('Ctrl Pts',(0.0179785702873004,0.145483266051774,
0.102587060617492));
#14040=CARTESIAN_POINT('Ctrl Pts',(0.0660590839964643,0.139541565957016,
0.0999407307383904));
#14041=CARTESIAN_POINT('Ctrl Pts',(0.110902718892925,0.107406914044162,
0.0972944008592884));
#14042=CARTESIAN_POINT('Ctrl Pts',(0.131983829661647,0.0637877973597534,
0.0946480709801865));
#14043=CARTESIAN_POINT('Ctrl Pts',(0.15306494043037,0.0201686806753445,
0.0920017411010846));
#14044=CARTESIAN_POINT('Ctrl Pts',(0.150383527071356,-0.0349349007806195,
0.0893554112219828));
#14045=CARTESIAN_POINT('Ctrl Pts',(0.125166930059577,-0.0763010783846813,
0.0867090813428809));
#14046=CARTESIAN_POINT('Ctrl Pts',(0.0999503330477985,-0.117667255988743,
0.084062751463779));
#14047=CARTESIAN_POINT('Ctrl Pts',(0.0521985523832557,-0.145296029740903,
0.081416421584677));
#14048=CARTESIAN_POINT('Ctrl Pts',(0.00376830011669856,-0.146541450754272,
0.0787700917055751));
#14049=CARTESIAN_POINT('Ctrl Pts',(-0.0446619521498586,-0.147786871767642,
0.0761237618264732));
#14050=CARTESIAN_POINT('Ctrl Pts',(-0.09377067601843,-0.122648940042221,
0.0734774319473713));
#14051=CARTESIAN_POINT('Ctrl Pts',(-0.121079980470766,-0.0826333491581908,
0.0708311020682694));
#14052=CARTESIAN_POINT('Ctrl Pts',(-0.137473143648068,-0.0586128871159229,
0.0692425695736098));
#14053=CARTESIAN_POINT('Ctrl Pts',(-0.146011252866834,-0.02923151094855,
0.0676540370789502));
#14054=CARTESIAN_POINT('Ctrl Pts',(-0.146148830924315,7.59978318484386E-5,
0.0660655045842905));
#14055=CARTESIAN_POINT('Ctrl Pts',(-0.146133770585873,6.2751561688711E-5,
0.0589344954157103));
#14056=CARTESIAN_POINT('Ctrl Pts',(-0.146026644150963,-0.0282514289199324,
0.0604687786045534));
#14057=CARTESIAN_POINT('Ctrl Pts',(-0.138100435392092,-0.0566215672018456,
0.0620030617933965));
#14058=CARTESIAN_POINT('Ctrl Pts',(-0.122745086057252,-0.0801407530065182,
0.0635373449822396));
#14059=CARTESIAN_POINT('Ctrl Pts',(-0.0962495935935968,-0.120722858737265,
0.0661847343564996));
#14060=CARTESIAN_POINT('Ctrl Pts',(-0.0476352194187008,-0.146862157398507,
0.0688321237307596));
#14061=CARTESIAN_POINT('Ctrl Pts',(0.00082938917649622,-0.146587691816784,
0.0714795131050196));
#14062=CARTESIAN_POINT('Ctrl Pts',(0.0492939977716932,-0.146313226235061,
0.0741269024792796));
#14063=CARTESIAN_POINT('Ctrl Pts',(0.0976088407871913,-0.119624996410372,
0.0767742918535397));
#14064=CARTESIAN_POINT('Ctrl Pts',(0.123643642180798,-0.0787464320231966,
0.0794216812277997));
#14065=CARTESIAN_POINT('Ctrl Pts',(0.149678443574405,-0.0378678676360213,
0.0820690706020596));
#14066=CARTESIAN_POINT('Ctrl Pts',(0.153433203346121,0.0172010313136401,
0.0847164599763195));
#14067=CARTESIAN_POINT('Ctrl Pts',(0.133187835944515,0.06123527443138,0.0873638493505795));
#14068=CARTESIAN_POINT('Ctrl Pts',(0.11294246854291,0.10526951754912,0.0900112387248395));
#14069=CARTESIAN_POINT('Ctrl Pts',(0.0686969739679828,0.138269104834938,
0.0926586280990997));
#14070=CARTESIAN_POINT('Ctrl Pts',(0.0207181735233275,0.145118849380084,
0.0953060174733597));
#14071=CARTESIAN_POINT('Ctrl Pts',(-0.027260626921328,0.151968593925229,
0.0979534068476197));
#14072=CARTESIAN_POINT('Ctrl Pts',(-0.0789727332357116,0.132668495729702,
0.10060079622188));
#14073=CARTESIAN_POINT('Ctrl Pts',(-0.110731403441959,0.0960588230543748,
0.10324818559614));
#14074=CARTESIAN_POINT('Ctrl Pts',(-0.133469481440122,0.0698475998711364,
0.105143622202663));
#14075=CARTESIAN_POINT('Ctrl Pts',(-0.145979327216774,0.0347634013028336,
0.107039058809187));
#14076=CARTESIAN_POINT('Ctrl Pts',(-0.146276374479508,-0.000129480650117819,
0.10893449541571));
#14077=CARTESIAN_POINT('Origin',(0.,0.,0.));
#14078=CARTESIAN_POINT('',(-0.146589818999335,-3.81787486967988E-6,0.166065504584291));
#14079=CARTESIAN_POINT('',(-0.146589453522336,1.04004190909306E-5,0.15893449541571));
#14080=CARTESIAN_POINT('',(-0.14635,-1.79227059055215E-17,0.));
#14081=CARTESIAN_POINT('Ctrl Pts',(-0.146589818999335,-3.81787486967988E-6,
0.166065504584291));
#14082=CARTESIAN_POINT('Ctrl Pts',(-0.146571339149733,0.0482382848470949,
0.163430332415738));
#14083=CARTESIAN_POINT('Ctrl Pts',(-0.120433071521034,0.0964975486977609,
0.160795160247185));
#14084=CARTESIAN_POINT('Ctrl Pts',(-0.0800107885095625,0.122828684230981,
0.158159988078632));
#14085=CARTESIAN_POINT('Ctrl Pts',(-0.0394173515450545,0.149271309704865,
0.15551365819953));
#14086=CARTESIAN_POINT('Ctrl Pts',(0.0155813181737399,0.153599719825856,
0.152867328320428));
#14087=CARTESIAN_POINT('Ctrl Pts',(0.0598114643267532,0.133832733731537,
0.150220998441327));
#14088=CARTESIAN_POINT('Ctrl Pts',(0.104041610479766,0.114065747637217,
0.147574668562225));
#14089=CARTESIAN_POINT('Ctrl Pts',(0.137503233066998,0.0702033653275883,
0.144928338683123));
#14090=CARTESIAN_POINT('Ctrl Pts',(0.144880420813362,0.0223220882221681,
0.142282008804021));
#14091=CARTESIAN_POINT('Ctrl Pts',(0.152257608559726,-0.0255591888832524,
0.139635678924919));
#14092=CARTESIAN_POINT('Ctrl Pts',(0.133550361465222,-0.077459360784464,
0.136989349045817));
#14093=CARTESIAN_POINT('Ctrl Pts',(0.0973212811704284,-0.109622900294719,
0.134343019166715));
#14094=CARTESIAN_POINT('Ctrl Pts',(0.0610922008756344,-0.141786439804975,
0.131696689287613));
#14095=CARTESIAN_POINT('Ctrl Pts',(0.00734128738055008,-0.154213346924274,
0.129050359408511));
#14096=CARTESIAN_POINT('Ctrl Pts',(-0.0393288211819405,-0.141215634503184,
0.126404029529409));
#14097=CARTESIAN_POINT('Ctrl Pts',(-0.0859989297444312,-0.128217922082094,
0.123757699650308));
#14098=CARTESIAN_POINT('Ctrl Pts',(-0.125588233374328,-0.0897955901206149,
0.121111369771206));
#14099=CARTESIAN_POINT('Ctrl Pts',(-0.139976083766172,-0.043535137330043,
0.118465039892104));
#14100=CARTESIAN_POINT('Ctrl Pts',(-0.144324767489921,-0.0295530571287048,
0.117665194789499));
#14101=CARTESIAN_POINT('Ctrl Pts',(-0.146371217526823,-0.0148549394177889,
0.116865349686895));
#14102=CARTESIAN_POINT('Ctrl Pts',(-0.146252097264499,-0.000124487410312429,
0.116065504584291));
#14103=CARTESIAN_POINT('Ctrl Pts',(-0.146276374479508,-0.000129480650117819,
0.10893449541571));
#14104=CARTESIAN_POINT('Ctrl Pts',(-0.14639421831063,-0.0139720956278579,
0.109686448183447));
#14105=CARTESIAN_POINT('Ctrl Pts',(-0.14458995413065,-0.0277846002915201,
0.110438400951183));
#14106=CARTESIAN_POINT('Ctrl Pts',(-0.140739671041232,-0.041001045008257,
0.11119035371892));
#14107=CARTESIAN_POINT('Ctrl Pts',(-0.127184034336146,-0.0875319932404337,
0.11383774309318));
#14108=CARTESIAN_POINT('Ctrl Pts',(-0.0882675268278623,-0.12667464254966,
0.11648513246744));
#14109=CARTESIAN_POINT('Ctrl Pts',(-0.0418159243469935,-0.140499695546946,
0.1191325218417));
#14110=CARTESIAN_POINT('Ctrl Pts',(0.00463567813387508,-0.154324748544231,
0.12177991121596));
#14111=CARTESIAN_POINT('Ctrl Pts',(0.0586223755873289,-0.142832205229577,
0.12442730059022));
#14112=CARTESIAN_POINT('Ctrl Pts',(0.0954154960694136,-0.111286216216264,
0.12707468996448));
#14113=CARTESIAN_POINT('Ctrl Pts',(0.132208616551499,-0.0797402272029501,
0.12972207933874));
#14114=CARTESIAN_POINT('Ctrl Pts',(0.151808160062214,-0.0281407924909768,
0.132369468712999));
#14115=CARTESIAN_POINT('Ctrl Pts',(0.145236524363737,0.0198768833792122,
0.135016858087259));
#14116=CARTESIAN_POINT('Ctrl Pts',(0.138664888665259,0.0678945592494009,
0.13766424746152));
#14117=CARTESIAN_POINT('Ctrl Pts',(0.105922073757589,0.112330476277805,
0.14031163683578));
#14118=CARTESIAN_POINT('Ctrl Pts',(0.062005973158836,0.132830708741579,
0.14295902621004));
#14119=CARTESIAN_POINT('Ctrl Pts',(0.0180898725600832,0.153330941205352,
0.1456064155843));
#14120=CARTESIAN_POINT('Ctrl Pts',(-0.0369995137297515,0.149895489104495,
0.14825380495856));
#14121=CARTESIAN_POINT('Ctrl Pts',(-0.0780284182758478,0.124097962381086,
0.15090119433282));
#14122=CARTESIAN_POINT('Ctrl Pts',(-0.119057322821944,0.0983004356576776,
0.153548583707079));
#14123=CARTESIAN_POINT('Ctrl Pts',(-0.146025745624302,0.0501408343117172,
0.15619597308134));
#14124=CARTESIAN_POINT('Ctrl Pts',(-0.14658076309025,0.00167873146180186,
0.1588433624556));
#14125=CARTESIAN_POINT('Ctrl Pts',(-0.146587131676737,0.00112264969450139,
0.15887374010897));
#14126=CARTESIAN_POINT('Ctrl Pts',(-0.146590022522527,0.000566528098114988,
0.15890411776234));
#14127=CARTESIAN_POINT('Ctrl Pts',(-0.146589453522336,1.04004190909306E-5,
0.15893449541571));
#14128=CARTESIAN_POINT('Origin',(0.,0.,0.));
#14129=CARTESIAN_POINT('',(-0.146263250741535,0.000126870157254357,0.21606550458429));
#14130=CARTESIAN_POINT('',(-0.146245769975643,0.000123264779366826,0.20893449541571));
#14131=CARTESIAN_POINT('',(-0.14635,-1.79227059055215E-17,0.));
#14132=CARTESIAN_POINT('Ctrl Pts',(-0.146263250741535,0.000126870157254357,
0.21606550458429));
#14133=CARTESIAN_POINT('Ctrl Pts',(-0.146381923100139,0.0144435832128767,
0.215287974902784));
#14134=CARTESIAN_POINT('Ctrl Pts',(-0.144450237714319,0.0287289633064517,
0.214510445221278));
#14135=CARTESIAN_POINT('Ctrl Pts',(-0.140337374518256,0.0423560295890773,
0.213732915539772));
#14136=CARTESIAN_POINT('Ctrl Pts',(-0.126339204386259,0.0887358830222778,
0.21108658566067));
#14137=CARTESIAN_POINT('Ctrl Pts',(-0.0870745347363382,0.127489909020004,
0.208440255781569));
#14138=CARTESIAN_POINT('Ctrl Pts',(-0.0405154226099946,0.140879780169064,
0.205793925902467));
#14139=CARTESIAN_POINT('Ctrl Pts',(0.00604368951634975,0.154269651318124,
0.203147596023365));
#14140=CARTESIAN_POINT('Ctrl Pts',(0.0598972441191175,0.142295367618517,
0.200501266144263));
#14141=CARTESIAN_POINT('Ctrl Pts',(0.0963956219934077,0.110437747119808,
0.197854936265161));
#14142=CARTESIAN_POINT('Ctrl Pts',(0.132893999867697,0.0785801266211,0.195208606386059));
#14143=CARTESIAN_POINT('Ctrl Pts',(0.15203720101351,0.0268391693232909,
0.192562276506957));
#14144=CARTESIAN_POINT('Ctrl Pts',(0.145063081087281,-0.0211024746124516,
0.189915946627855));
#14145=CARTESIAN_POINT('Ctrl Pts',(0.138088961161051,-0.0690441185481943,
0.187269616748753));
#14146=CARTESIAN_POINT('Ctrl Pts',(0.10499752016278,-0.11318644912187,0.184623286869651));
#14147=CARTESIAN_POINT('Ctrl Pts',(0.060935231264163,-0.133324827106958,
0.181976956990549));
#14148=CARTESIAN_POINT('Ctrl Pts',(0.0168729423655461,-0.153463205092045,
0.179330627111448));
#14149=CARTESIAN_POINT('Ctrl Pts',(-0.0381601944334158,-0.149597630488544,
0.176684297232346));
#14150=CARTESIAN_POINT('Ctrl Pts',(-0.0789746466099193,-0.123497437688695,
0.174037967353244));
#14151=CARTESIAN_POINT('Ctrl Pts',(-0.119961184605052,-0.0972871987457574,
0.171380479763593));
#14152=CARTESIAN_POINT('Ctrl Pts',(-0.146608455341797,-0.0486544490602708,
0.168722992173942));
#14153=CARTESIAN_POINT('Ctrl Pts',(-0.146589818999335,-3.81787486967988E-6,
0.166065504584291));
#14154=CARTESIAN_POINT('Ctrl Pts',(-0.146589453522336,1.04004190909306E-5,
0.15893449541571));
#14155=CARTESIAN_POINT('Ctrl Pts',(-0.146540434588914,-0.0478995759235739,
0.1615515071366));
#14156=CARTESIAN_POINT('Ctrl Pts',(-0.120813506558866,-0.0958546957256878,
0.16416851885749));
#14157=CARTESIAN_POINT('Ctrl Pts',(-0.0808500697395765,-0.122278388912248,
0.16678553057838));
#14158=CARTESIAN_POINT('Ctrl Pts',(-0.0404227467934142,-0.149008802082514,
0.16943291995264));
#14159=CARTESIAN_POINT('Ctrl Pts',(0.0145735112284506,-0.153705024069172,
0.1720803093269));
#14160=CARTESIAN_POINT('Ctrl Pts',(0.0589475933459444,-0.134215943447351,
0.17472769870116));
#14161=CARTESIAN_POINT('Ctrl Pts',(0.103321675463438,-0.11472686282553,
0.17737508807542));
#14162=CARTESIAN_POINT('Ctrl Pts',(0.137073581676561,-0.0710524795952304,
0.18002247744968));
#14163=CARTESIAN_POINT('Ctrl Pts',(0.144743205110219,-0.0231979049720499,
0.18266986682394));
#14164=CARTESIAN_POINT('Ctrl Pts',(0.152412828543877,0.024656669651131,
0.1853172561982));
#14165=CARTESIAN_POINT('Ctrl Pts',(0.13400016919807,0.0766914356671922,
0.18796464557246));
#14166=CARTESIAN_POINT('Ctrl Pts',(0.0979391709064228,0.109071797518936,
0.19061203494672));
#14167=CARTESIAN_POINT('Ctrl Pts',(0.0618781726147763,0.141452159370678,
0.19325942432098));
#14168=CARTESIAN_POINT('Ctrl Pts',(0.00816883537729064,0.154178117058104,
0.195906813695239));
#14169=CARTESIAN_POINT('Ctrl Pts',(-0.0385872054932313,0.1414205281901,
0.198554203069499));
#14170=CARTESIAN_POINT('Ctrl Pts',(-0.0853432463637543,0.128662939322095,
0.201201592443759));
#14171=CARTESIAN_POINT('Ctrl Pts',(-0.125145990867313,0.0904218038986596,
0.20384898181802));
#14172=CARTESIAN_POINT('Ctrl Pts',(-0.139763737461459,0.0442135263146365,
0.20649637119228));
#14173=CARTESIAN_POINT('Ctrl Pts',(-0.144251162244238,0.030028291356252,
0.207309079266757));
#14174=CARTESIAN_POINT('Ctrl Pts',(-0.146365162502875,0.0150922359825044,
0.208121787341234));
#14175=CARTESIAN_POINT('Ctrl Pts',(-0.146245769975643,0.000123264779366826,
0.20893449541571));
#14176=CARTESIAN_POINT('Origin',(0.,0.,0.));
#14177=CARTESIAN_POINT('',(-0.146142672279203,-7.01165389862951E-5,0.266065504584291));
#14178=CARTESIAN_POINT('',(-0.146150215784492,-7.74481165901552E-5,0.258934495415711));
#14179=CARTESIAN_POINT('',(-0.14635,-1.79227059055215E-17,0.));
#14180=CARTESIAN_POINT('Ctrl Pts',(-0.146142672279203,-7.01165389862951E-5,
0.266065504584291));
#14181=CARTESIAN_POINT('Ctrl Pts',(-0.146017527260215,0.028828671850369,
0.264499287510729));
#14182=CARTESIAN_POINT('Ctrl Pts',(-0.137733916992107,0.0577936173630845,
0.262933070437168));
#14183=CARTESIAN_POINT('Ctrl Pts',(-0.121770841384076,0.0816117278206753,
0.261366853363607));
#14184=CARTESIAN_POINT('Ctrl Pts',(-0.0947991242083451,0.121855560193383,
0.258720523484505));
#14185=CARTESIAN_POINT('Ctrl Pts',(-0.0459036471244643,0.147405924851771,
0.256074193605403));
#14186=CARTESIAN_POINT('Ctrl Pts',(0.0025353607453442,0.146568017913755,
0.253427863726301));
#14187=CARTESIAN_POINT('Ctrl Pts',(0.050974368615152,0.145730110975738,
0.250781533847199));
#14188=CARTESIAN_POINT('Ctrl Pts',(0.0989569072708876,0.118503932441319,
0.248135203968097));
#14189=CARTESIAN_POINT('Ctrl Pts',(0.124520613871998,0.0773513325689396,
0.245488874088995));
#14190=CARTESIAN_POINT('Ctrl Pts',(0.150084320473109,0.0361987326965595,
0.242842544209893));
#14191=CARTESIAN_POINT('Ctrl Pts',(0.153229195019594,-0.0188802885137813,
0.240196214330791));
#14192=CARTESIAN_POINT('Ctrl Pts',(0.132515778953886,-0.0626751965094481,
0.237549884451689));
#14193=CARTESIAN_POINT('Ctrl Pts',(0.111802362888177,-0.106470104505115,
0.234903554572587));
#14194=CARTESIAN_POINT('Ctrl Pts',(0.0672306562102751,-0.138980899286108,
0.232257224693486));
#14195=CARTESIAN_POINT('Ctrl Pts',(0.0192018303028616,-0.145326878595667,
0.229610894814384));
#14196=CARTESIAN_POINT('Ctrl Pts',(-0.0288269956045516,-0.151672857905225,
0.226964564935282));
#14197=CARTESIAN_POINT('Ctrl Pts',(-0.0803129407414762,-0.131854021743351,
0.22431823505618));
#14198=CARTESIAN_POINT('Ctrl Pts',(-0.111690078002902,-0.0949417632280756,
0.221671905177078));
#14199=CARTESIAN_POINT('Ctrl Pts',(-0.133848162215005,-0.0688748557907962,
0.219803104979482));
#14200=CARTESIAN_POINT('Ctrl Pts',(-0.145978020566425,-0.0342834897603843,
0.217934304781886));
#14201=CARTESIAN_POINT('Ctrl Pts',(-0.146263250741535,0.000126870157254357,
0.21606550458429));
#14202=CARTESIAN_POINT('Ctrl Pts',(-0.146245769975643,0.000123264779366826,
0.20893449541571));
#14203=CARTESIAN_POINT('Ctrl Pts',(-0.145976242399967,-0.03366905549635,
0.210769176715493));
#14204=CARTESIAN_POINT('Ctrl Pts',(-0.134324750276972,-0.067629123606452,
0.212603858015276));
#14205=CARTESIAN_POINT('Ctrl Pts',(-0.112902327433,-0.0934976078712483,
0.214438539315059));
#14206=CARTESIAN_POINT('Ctrl Pts',(-0.0819904221256615,-0.130825044728502,
0.217085928689319));
#14207=CARTESIAN_POINT('Ctrl Pts',(-0.0307338628262512,-0.151304498698398,
0.21973331806358));
#14208=CARTESIAN_POINT('Ctrl Pts',(0.0173892134168267,-0.145555327884408,
0.22238070743784));
#14209=CARTESIAN_POINT('Ctrl Pts',(0.0655122896599044,-0.139806157070418,
0.2250280968121));
#14210=CARTESIAN_POINT('Ctrl Pts',(0.11050188284665,-0.107828361472542,
0.22767548618636));
#14211=CARTESIAN_POINT('Ctrl Pts',(0.131750448317205,-0.0642694140823833,
0.23032287556062));
#14212=CARTESIAN_POINT('Ctrl Pts',(0.15299901378776,-0.020710466692225,
0.232970264934879));
#14213=CARTESIAN_POINT('Ctrl Pts',(0.150506551542124,0.0344296324902152,
0.23561765430914));
#14214=CARTESIAN_POINT('Ctrl Pts',(0.125414737320077,0.0758938856636754,
0.2382650436834));
#14215=CARTESIAN_POINT('Ctrl Pts',(0.10032292309803,0.117358138837136,0.24091243305766));
#14216=CARTESIAN_POINT('Ctrl Pts',(0.0526317568995709,0.145146546001616,
0.24355982243192));
#14217=CARTESIAN_POINT('Ctrl Pts',(0.00418624259284972,0.146530589268381,
0.24620721180618));
#14218=CARTESIAN_POINT('Ctrl Pts',(-0.0442592717138715,0.147914632535146,
0.24885460118044));
#14219=CARTESIAN_POINT('Ctrl Pts',(-0.0934591341288551,0.122894311904195,
0.2515019905547));
#14220=CARTESIAN_POINT('Ctrl Pts',(-0.120877280418781,0.082930219442967,
0.25414937992896));
#14221=CARTESIAN_POINT('Ctrl Pts',(-0.137396572682769,0.0588520590724165,
0.255744418424543));
#14222=CARTESIAN_POINT('Ctrl Pts',(-0.146009100715185,0.0293493086505574,
0.257339456920127));
#14223=CARTESIAN_POINT('Ctrl Pts',(-0.146150215784492,-7.74481165901552E-5,
0.258934495415711));
#14224=CARTESIAN_POINT('Origin',(0.,0.,0.));
#14225=CARTESIAN_POINT('',(-0.146519404976022,-8.97763884284003E-5,0.316065504584291));
#14226=CARTESIAN_POINT('',(-0.146528765763263,-8.45393868379275E-5,0.30893449541571));
#14227=CARTESIAN_POINT('',(-0.14635,-1.79227059055215E-17,0.));
#14228=CARTESIAN_POINT('Ctrl Pts',(-0.146519404976022,-8.97763884284003E-5,
0.316065504584291));
#14229=CARTESIAN_POINT('Ctrl Pts',(-0.146208092107557,0.043076445171776,
0.313710600118674));
#14230=CARTESIAN_POINT('Ctrl Pts',(-0.125958424314353,0.0864965766126209,
0.311355695653057));
#14231=CARTESIAN_POINT('Ctrl Pts',(-0.0925183485457987,0.1137056160074,
0.309000791187441));
#14232=CARTESIAN_POINT('Ctrl Pts',(-0.0549399784004991,0.144281843189175,
0.306354461308339));
#14233=CARTESIAN_POINT('Ctrl Pts',(-0.00070450021881692,0.154386382754941,
0.303708131429237));
#14234=CARTESIAN_POINT('Ctrl Pts',(0.0453636543616171,0.139394227973128,
0.301061801550135));
#14235=CARTESIAN_POINT('Ctrl Pts',(0.0914318089420511,0.124402073191315,
0.298415471671033));
#14236=CARTESIAN_POINT('Ctrl Pts',(0.129332639921237,0.0843132240619223,
0.295769141791931));
#14237=CARTESIAN_POINT('Ctrl Pts',(0.141718340675246,0.0374769775398043,
0.293122811912829));
#14238=CARTESIAN_POINT('Ctrl Pts',(0.154104041429255,-0.00935926898231351,
0.290476482033727));
#14239=CARTESIAN_POINT('Ctrl Pts',(0.140974611958088,-0.0629429128971569,
0.287830152154626));
#14240=CARTESIAN_POINT('Ctrl Pts',(0.108339598692885,-0.0987478773661917,
0.285183822275524));
#14241=CARTESIAN_POINT('Ctrl Pts',(0.0757045854276824,-0.134552841835227,
0.282537492396422));
#14242=CARTESIAN_POINT('Ctrl Pts',(0.0235639883684441,-0.152579126858453,
0.27989116251732));
#14243=CARTESIAN_POINT('Ctrl Pts',(-0.0242166208952047,-0.144575818177467,
0.277244832638218));
#14244=CARTESIAN_POINT('Ctrl Pts',(-0.0719972301588528,-0.136572509496481,
0.274598502759116));
#14245=CARTESIAN_POINT('Ctrl Pts',(-0.115417851626912,-0.102539607111283,
0.271952172880014));
#14246=CARTESIAN_POINT('Ctrl Pts',(-0.13460418372715,-0.0580545058751705,
0.269305843000912));
#14247=CARTESIAN_POINT('Ctrl Pts',(-0.142435181350113,-0.0398976888130428,
0.268225730195372));
#14248=CARTESIAN_POINT('Ctrl Pts',(-0.146228976240411,-0.0199996345674016,
0.267145617389831));
#14249=CARTESIAN_POINT('Ctrl Pts',(-0.146142672279203,-7.01165389862951E-5,
0.266065504584291));
#14250=CARTESIAN_POINT('Ctrl Pts',(-0.146150215784492,-7.74481165901552E-5,
0.258934495415711));
#14251=CARTESIAN_POINT('Ctrl Pts',(-0.146243318595233,-0.0194921979337541,
0.259986846294387));
#14252=CARTESIAN_POINT('Ctrl Pts',(-0.142648899141753,-0.0388738684647463,
0.261039197173063));
#14253=CARTESIAN_POINT('Ctrl Pts',(-0.135204796371803,-0.0566427511368837,
0.26209154805174));
#14254=CARTESIAN_POINT('Ctrl Pts',(-0.116477735870028,-0.101343764964001,
0.264738937426));
#14255=CARTESIAN_POINT('Ctrl Pts',(-0.0733871847016099,-0.135837928326728,
0.26738632680026));
#14256=CARTESIAN_POINT('Ctrl Pts',(-0.0256708287318585,-0.144325142544676,
0.27003371617452));
#14257=CARTESIAN_POINT('Ctrl Pts',(0.0220455272378925,-0.152812356762624,
0.27268110554878));
#14258=CARTESIAN_POINT('Ctrl Pts',(0.0743876880089763,-0.135292621835792,
0.27532849492304));
#14259=CARTESIAN_POINT('Ctrl Pts',(0.10738025529095,-0.0997908762961729,
0.2779758842973));
#14260=CARTESIAN_POINT('Ctrl Pts',(0.140372822572925,-0.0642891307565533,
0.280623273671559));
#14261=CARTESIAN_POINT('Ctrl Pts',(0.154015796365789,-0.010805374604146,
0.283270663045819));
#14262=CARTESIAN_POINT('Ctrl Pts',(0.142059993874458,0.0361620845457957,
0.285918052420079));
#14263=CARTESIAN_POINT('Ctrl Pts',(0.130104191383128,0.0831295436957373,
0.288565441794339));
#14264=CARTESIAN_POINT('Ctrl Pts',(0.0925496126076039,0.123580705843213,
0.291212831168599));
#14265=CARTESIAN_POINT('Ctrl Pts',(0.0465981836912963,0.138986860871753,
0.29386022054286));
#14266=CARTESIAN_POINT('Ctrl Pts',(0.000646754774988913,0.154393015900293,
0.296507609917119));
#14267=CARTESIAN_POINT('Ctrl Pts',(-0.0537015242821025,0.144754163809898,
0.29915499929138));
#14268=CARTESIAN_POINT('Ctrl Pts',(-0.0915523499663989,0.114485393976436,
0.30180238866564));
#14269=CARTESIAN_POINT('Ctrl Pts',(-0.125542580994678,0.0873038870745135,
0.30417975758233));
#14270=CARTESIAN_POINT('Ctrl Pts',(-0.146229051243382,0.0434861464246214,
0.30655712649902));
#14271=CARTESIAN_POINT('Ctrl Pts',(-0.146528765763263,-8.45393868379275E-5,
0.30893449541571));
#14272=CARTESIAN_POINT('Origin',(0.,0.,0.));
#14273=CARTESIAN_POINT('',(-0.146416087288192,0.000126442170093593,0.366065504584291));
#14274=CARTESIAN_POINT('',(-0.146408012399712,0.000128195943346294,0.358934495415711));
#14275=CARTESIAN_POINT('',(-0.14635,-1.79227059055215E-17,0.));
#14276=CARTESIAN_POINT('Ctrl Pts',(-0.146416087288192,0.000126442170093593,
0.366065504584291));
#14277=CARTESIAN_POINT('Ctrl Pts',(-0.146499294961499,0.00925816812376314,
0.365568242605721));
#14278=CARTESIAN_POINT('Ctrl Pts',(-0.145718277739785,0.0183757049974218,
0.365070980627151));
#14279=CARTESIAN_POINT('Ctrl Pts',(-0.144021710151773,0.0273195705351122,
0.364573718648581));
#14280=CARTESIAN_POINT('Ctrl Pts',(-0.134992913071845,0.0749170536065741,
0.361927388769479));
#14281=CARTESIAN_POINT('Ctrl Pts',(-0.100034284522917,0.117595890322328,
0.359281058890377));
#14282=CARTESIAN_POINT('Ctrl Pts',(-0.0551469387876206,0.135821305661589,
0.356634729011275));
#14283=CARTESIAN_POINT('Ctrl Pts',(-0.0102595930523245,0.15404672100085,
0.353988399132173));
#14284=CARTESIAN_POINT('Ctrl Pts',(0.0445564698693406,0.147818714963618,
0.351342069253072));
#14285=CARTESIAN_POINT('Ctrl Pts',(0.0842110755700531,0.119987943896873,
0.34869573937397));
#14286=CARTESIAN_POINT('Ctrl Pts',(0.123865681270766,0.0921571728301272,
0.346049409494868));
#14287=CARTESIAN_POINT('Ctrl Pts',(0.148358829750526,0.0427236367338667,
0.343403079615766));
#14288=CARTESIAN_POINT('Ctrl Pts',(0.146479621605269,-0.00568615719458776,
0.340756749736664));
#14289=CARTESIAN_POINT('Ctrl Pts',(0.144600413460012,-0.0540959511230416,
0.338110419857562));
#14290=CARTESIAN_POINT('Ctrl Pts',(0.116348848689739,-0.101482002883689,
0.33546408997846));
#14291=CARTESIAN_POINT('Ctrl Pts',(0.0746561129649502,-0.126154971072205,
0.332817760099358));
#14292=CARTESIAN_POINT('Ctrl Pts',(0.0329633772401616,-0.150827939260721,
0.330171430220256));
#14293=CARTESIAN_POINT('Ctrl Pts',(-0.0221705294391424,-0.152787823877104,
0.327525100341154));
#14294=CARTESIAN_POINT('Ctrl Pts',(-0.0655099505772086,-0.131137554898038,
0.324878770462052));
#14295=CARTESIAN_POINT('Ctrl Pts',(-0.108849371715275,-0.109487285918972,
0.322232440582951));
#14296=CARTESIAN_POINT('Ctrl Pts',(-0.140394307312104,-0.0642268633444555,
0.319586110703849));
#14297=CARTESIAN_POINT('Ctrl Pts',(-0.14570614405606,-0.0160726946583056,
0.316939780824747));
#14298=CARTESIAN_POINT('Ctrl Pts',(-0.146291106736525,-0.0107697471190636,
0.316648355411261));
#14299=CARTESIAN_POINT('Ctrl Pts',(-0.146557930734812,-0.0054317060295066,
0.316356929997776));
#14300=CARTESIAN_POINT('Ctrl Pts',(-0.146519404976022,-8.97763884284003E-5,
0.316065504584291));
#14301=CARTESIAN_POINT('Ctrl Pts',(-0.146528765763263,-8.45393868379275E-5,
0.30893449541571));
#14302=CARTESIAN_POINT('Ctrl Pts',(-0.146562807199252,-0.00503327764821679,
0.30920451587328));
#14303=CARTESIAN_POINT('Ctrl Pts',(-0.14633385314783,-0.00997882882536714,
0.30947453633085));
#14304=CARTESIAN_POINT('Ctrl Pts',(-0.145831525524598,-0.0148964553326841,
0.309744556788419));
#14305=CARTESIAN_POINT('Ctrl Pts',(-0.140906503086998,-0.0631108472318147,
0.312391946162679));
#14306=CARTESIAN_POINT('Ctrl Pts',(-0.109703085900295,-0.108640943453547,
0.31503933553694));
#14307=CARTESIAN_POINT('Ctrl Pts',(-0.0665140418604196,-0.13063162118607,
0.3176867249112));
#14308=CARTESIAN_POINT('Ctrl Pts',(-0.0233249978205455,-0.152622298918592,
0.32033411428546));
#14309=CARTESIAN_POINT('Ctrl Pts',(0.0318496730725009,-0.151073558161906,
0.322981503659719));
#14310=CARTESIAN_POINT('Ctrl Pts',(0.0737371373950496,-0.126694801736668,
0.325628893033979));
#14311=CARTESIAN_POINT('Ctrl Pts',(0.115624601717599,-0.10231604531143,
0.328276282408239));
#14312=CARTESIAN_POINT('Ctrl Pts',(0.144224859469651,-0.0551072732176397,
0.3309236717825));
#14313=CARTESIAN_POINT('Ctrl Pts',(0.146437523492708,-0.0066925280449658,
0.33357106115676));
#14314=CARTESIAN_POINT('Ctrl Pts',(0.148650187515766,0.0417222171277085,
0.33621845053102));
#14315=CARTESIAN_POINT('Ctrl Pts',(0.124475257809829,0.0913429353792657,
0.33886583990528));
#14316=CARTESIAN_POINT('Ctrl Pts',(0.0849860939726622,0.119440788885456,
0.34151322927954));
#14317=CARTESIAN_POINT('Ctrl Pts',(0.0454969301354961,0.147538642391646,
0.344160618653799));
#14318=CARTESIAN_POINT('Ctrl Pts',(-0.00930646783289898,0.154113631152469,
0.346808008028059));
#14319=CARTESIAN_POINT('Ctrl Pts',(-0.0543213285795041,0.136154072578339,
0.349455397402319));
#14320=CARTESIAN_POINT('Ctrl Pts',(-0.0993361893261098,0.11819451400421,
0.352102786776579));
#14321=CARTESIAN_POINT('Ctrl Pts',(-0.134562512850926,0.0757004080951257,
0.35475017615084));
#14322=CARTESIAN_POINT('Ctrl Pts',(-0.143864833510727,0.0281362381501331,
0.3573975655251));
#14323=CARTESIAN_POINT('Ctrl Pts',(-0.145664973529558,0.0189318504589563,
0.357909875488637));
#14324=CARTESIAN_POINT('Ctrl Pts',(-0.146494308508217,0.00953759842677947,
0.358422185452174));
#14325=CARTESIAN_POINT('Ctrl Pts',(-0.146408012399712,0.000128195943346294,
0.358934495415711));
#14326=CARTESIAN_POINT('Origin',(0.,0.,0.));
#14327=CARTESIAN_POINT('',(-0.146110491840834,1.12683595067248E-5,0.416065504584291));
#14328=CARTESIAN_POINT('',(-0.146109756335714,8.81622270207575E-6,0.40893449541571));
#14329=CARTESIAN_POINT('',(-0.14635,-1.79227059055215E-17,0.));
#14330=CARTESIAN_POINT('Ctrl Pts',(-0.146110491840834,1.12683595067248E-5,
0.416065504584291));
#14331=CARTESIAN_POINT('Ctrl Pts',(-0.146126798292857,0.0237518011834032,
0.414779555213666));
#14332=CARTESIAN_POINT('Ctrl Pts',(-0.140669750958991,0.0474852665485293,
0.413493605843041));
#14333=CARTESIAN_POINT('Ctrl Pts',(-0.129698698951591,0.0683144158983218,
0.412207656472415));
#14334=CARTESIAN_POINT('Ctrl Pts',(-0.107121587134001,0.111178312051432,
0.409561326593314));
#14335=CARTESIAN_POINT('Ctrl Pts',(-0.0611933749717542,0.141742803557285,
0.406914996714211));
#14336=CARTESIAN_POINT('Ctrl Pts',(-0.0129361277491455,0.146018041789781,
0.40426866683511));
#14337=CARTESIAN_POINT('Ctrl Pts',(0.0353211194734639,0.150293280022276,
0.401622336956008));
#14338=CARTESIAN_POINT('Ctrl Pts',(0.0859074017564354,0.128279264981412,
0.398976007076906));
#14339=CARTESIAN_POINT('Ctrl Pts',(0.115668581836909,0.0900521576926538,
0.396329677197804));
#14340=CARTESIAN_POINT('Ctrl Pts',(0.145429761917382,0.0518250504038959,
0.393683347318702));
#14341=CARTESIAN_POINT('Ctrl Pts',(0.154365839795359,-0.0026151491327561,
0.3910370174396));
#14342=CARTESIAN_POINT('Ctrl Pts',(0.138386632036901,-0.0483503050946702,
0.388390687560498));
#14343=CARTESIAN_POINT('Ctrl Pts',(0.122407424278443,-0.094085461056585,
0.385744357681396));
#14344=CARTESIAN_POINT('Ctrl Pts',(0.0815129308835505,-0.131115573443762,
0.383098027802294));
#14345=CARTESIAN_POINT('Ctrl Pts',(0.0344212048624006,-0.142491377230642,
0.380451697923192));
#14346=CARTESIAN_POINT('Ctrl Pts',(-0.0126705211587486,-0.153867181017521,
0.37780536804409));
#14347=CARTESIAN_POINT('Ctrl Pts',(-0.0659594798061549,-0.139588676204105,
0.375159038164988));
#14348=CARTESIAN_POINT('Ctrl Pts',(-0.101054476324393,-0.106191359083811,
0.372512708285887));
#14349=CARTESIAN_POINT('Ctrl Pts',(-0.129554902927378,-0.0790696072742943,
0.370363640385355));
#14350=CARTESIAN_POINT('Ctrl Pts',(-0.146056480184715,-0.0393390709180539,
0.368214572484823));
#14351=CARTESIAN_POINT('Ctrl Pts',(-0.146416087288192,0.000126442170093593,
0.366065504584291));
#14352=CARTESIAN_POINT('Ctrl Pts',(-0.146408012399712,0.000128195943346294,
0.358934495415711));
#14353=CARTESIAN_POINT('Ctrl Pts',(-0.146048368712081,-0.0390859965171687,
0.361069574826434));
#14354=CARTESIAN_POINT('Ctrl Pts',(-0.1297855810823,-0.0785633296797545,
0.363204654237157));
#14355=CARTESIAN_POINT('Ctrl Pts',(-0.101613371150224,-0.105657280969165,
0.36533973364788));
#14356=CARTESIAN_POINT('Ctrl Pts',(-0.066681270335132,-0.139252396162569,
0.36798712302214));
#14357=CARTESIAN_POINT('Ctrl Pts',(-0.0134387509101597,-0.153808392568477,
0.370634512396399));
#14358=CARTESIAN_POINT('Ctrl Pts',(0.0337263783221333,-0.142657876135818,
0.373281901770659));
#14359=CARTESIAN_POINT('Ctrl Pts',(0.0808915075544263,-0.13150735970316,
0.375929291144919));
#14360=CARTESIAN_POINT('Ctrl Pts',(0.12197924659404,-0.0946503304319347,
0.378576680519179));
#14361=CARTESIAN_POINT('Ctrl Pts',(0.138169300408926,-0.0489692009616054,
0.38122406989344));
#14362=CARTESIAN_POINT('Ctrl Pts',(0.154359354223812,-0.00328807149127619,
0.3838714592677));
#14363=CARTESIAN_POINT('Ctrl Pts',(0.14565172281397,0.0512171581781573,
0.38651884864196));
#14364=CARTESIAN_POINT('Ctrl Pts',(0.11603494864959,0.0895802930905963,
0.38916623801622));
#14365=CARTESIAN_POINT('Ctrl Pts',(0.0864181744852101,0.127943428003035,
0.39181362739048));
#14366=CARTESIAN_POINT('Ctrl Pts',(0.0358922575662923,0.15016446815848,
0.394461016764739));
#14367=CARTESIAN_POINT('Ctrl Pts',(-0.0123993367959677,0.146065035738641,
0.397108406138999));
#14368=CARTESIAN_POINT('Ctrl Pts',(-0.0606909311582276,0.141965603318802,
0.399755795513259));
#14369=CARTESIAN_POINT('Ctrl Pts',(-0.106748202963829,0.111545698323679,
0.40240318488752));
#14370=CARTESIAN_POINT('Ctrl Pts',(-0.129474555904152,0.0687391998188283,
0.40505057426178));
#14371=CARTESIAN_POINT('Ctrl Pts',(-0.140588317483115,0.0478057390183907,
0.406345214646423));
#14372=CARTESIAN_POINT('Ctrl Pts',(-0.146122589096428,0.0239100770892618,
0.407639855031067));
#14373=CARTESIAN_POINT('Ctrl Pts',(-0.146109756335714,8.81622270207575E-6,
0.40893449541571));
#14374=CARTESIAN_POINT('Origin',(0.,0.,0.));
#14375=CARTESIAN_POINT('',(-0.146374718215768,-0.000132229735885947,0.466065504584291));
#14376=CARTESIAN_POINT('',(-0.146375609273197,-0.000132432188538665,0.458934495415711));
#14377=CARTESIAN_POINT('',(-0.14635,-1.79227059055215E-17,0.));
#14378=CARTESIAN_POINT('Ctrl Pts',(-0.146374718215768,-0.000132229735885947,
0.466065504584291));
#14379=CARTESIAN_POINT('Ctrl Pts',(-0.146022504084922,0.0379941335185874,
0.46399086782161));
#14380=CARTESIAN_POINT('Ctrl Pts',(-0.130761950520226,0.0763703265456945,
0.46191623105893));
#14381=CARTESIAN_POINT('Ctrl Pts',(-0.103994021541854,0.103314352404769,
0.45984159429625));
#14382=CARTESIAN_POINT('Ctrl Pts',(-0.0698498419286355,0.137683154682254,
0.457195264417148));
#14383=CARTESIAN_POINT('Ctrl Pts',(-0.0169824611430249,0.153451124186949,
0.454548934538046));
#14384=CARTESIAN_POINT('Ctrl Pts',(0.030409888879481,0.143401013202843,
0.451902604658944));
#14385=CARTESIAN_POINT('Ctrl Pts',(0.0778022389019875,0.133350902218736,
0.449256274779842));
#14386=CARTESIAN_POINT('Ctrl Pts',(0.119719558161389,0.0974827107458278,
0.44660994490074));
#14387=CARTESIAN_POINT('Ctrl Pts',(0.136975630157447,0.0522138743269898,
0.443963615021638));
#14388=CARTESIAN_POINT('Ctrl Pts',(0.154231702153504,0.00694503790815254,
0.441317285142536));
#14389=CARTESIAN_POINT('Ctrl Pts',(0.146826526886218,-0.0477244434566137,
0.438670955263434));
#14390=CARTESIAN_POINT('Ctrl Pts',(0.118149569579287,-0.0867714880447125,
0.436024625384332));
#14391=CARTESIAN_POINT('Ctrl Pts',(0.0894726122723542,-0.125818532632812,
0.43337829550523));
#14392=CARTESIAN_POINT('Ctrl Pts',(0.0395238729257754,-0.149243140444243,
0.430731965626129));
#14393=CARTESIAN_POINT('Ctrl Pts',(-0.00883432462988853,-0.146323499949933,
0.428085635747027));
#14394=CARTESIAN_POINT('Ctrl Pts',(-0.0571925221855517,-0.143403859455623,
0.425439305867925));
#14395=CARTESIAN_POINT('Ctrl Pts',(-0.1039601779503,-0.114139970655572,
0.422792975988823));
#14396=CARTESIAN_POINT('Ctrl Pts',(-0.127731000096207,-0.0719263758553634,
0.420146646109721));
#14397=CARTESIAN_POINT('Ctrl Pts',(-0.139950702323481,-0.0502259249733931,
0.418786265601244));
#14398=CARTESIAN_POINT('Ctrl Pts',(-0.146093241566443,-0.0251033736724598,
0.417425885092767));
#14399=CARTESIAN_POINT('Ctrl Pts',(-0.146110491840834,1.12683595067248E-5,
0.416065504584291));
#14400=CARTESIAN_POINT('Ctrl Pts',(-0.146109756335714,8.81622270207575E-6,
0.40893449541571));
#14401=CARTESIAN_POINT('Ctrl Pts',(-0.146096347589706,-0.0249652282079418,
0.410287244405327));
#14402=CARTESIAN_POINT('Ctrl Pts',(-0.140026707259891,-0.049945385460595,
0.411639993394943));
#14403=CARTESIAN_POINT('Ctrl Pts',(-0.127937780377622,-0.0715588049813403,
0.412992742384559));
#14404=CARTESIAN_POINT('Ctrl Pts',(-0.104279217835726,-0.113857219262079,
0.415640131758819));
#14405=CARTESIAN_POINT('Ctrl Pts',(-0.0575666586768896,-0.14326095580898,
0.41828752113308));
#14406=CARTESIAN_POINT('Ctrl Pts',(-0.00919685447762893,-0.146301592903247,
0.42093491050734));
#14407=CARTESIAN_POINT('Ctrl Pts',(0.039172949721632,-0.149342229997515,
0.4235822998816));
#14408=CARTESIAN_POINT('Ctrl Pts',(0.089199998961318,-0.126019767639148,
0.426229689255859));
#14409=CARTESIAN_POINT('Ctrl Pts',(0.117969334952632,-0.0870170915920772,
0.428877078630119));
#14410=CARTESIAN_POINT('Ctrl Pts',(0.146738670943946,-0.0480144155450057,
0.431524468004379));
#14411=CARTESIAN_POINT('Ctrl Pts',(0.154250293686888,0.00666847419077017,
0.43417185737864));
#14412=CARTESIAN_POINT('Ctrl Pts',(0.137063494116028,0.051984005222912,
0.4368192467529));
#14413=CARTESIAN_POINT('Ctrl Pts',(0.119876694545168,0.0972995362550541,
0.43946663612716));
#14414=CARTESIAN_POINT('Ctrl Pts',(0.0779914726605056,0.133247708583562,
0.442114025501419));
#14415=CARTESIAN_POINT('Ctrl Pts',(0.0305934116013849,0.143362412733947,
0.444761414875679));
#14416=CARTESIAN_POINT('Ctrl Pts',(-0.0168046494577345,0.153477116884331,
0.447408804249939));
#14417=CARTESIAN_POINT('Ctrl Pts',(-0.0697155496913122,0.137758352856595,
0.4500561936242));
#14418=CARTESIAN_POINT('Ctrl Pts',(-0.103903378920715,0.103406122000434,
0.45270358299846));
#14419=CARTESIAN_POINT('Ctrl Pts',(-0.130724942802416,0.0764555792150183,
0.45478055380421));
#14420=CARTESIAN_POINT('Ctrl Pts',(-0.146022533856355,0.0380362146017157,
0.45685752460996));
#14421=CARTESIAN_POINT('Ctrl Pts',(-0.146375609273197,-0.000132432188538665,
0.458934495415711));
#14422=CARTESIAN_POINT('Origin',(0.,0.,0.));
#14423=CARTESIAN_POINT('',(-0.146548608312775,6.99729089778146E-5,0.516065504584291));
#14424=CARTESIAN_POINT('',(-0.146550766805835,6.86360251013434E-5,0.508934495415711));
#14425=CARTESIAN_POINT('',(-0.14635,-1.79227059055215E-17,0.));
#14426=CARTESIAN_POINT('Ctrl Pts',(-0.146548608312775,6.99729089778146E-5,
0.516065504584291));
#14427=CARTESIAN_POINT('Ctrl Pts',(-0.146572081366671,0.00404546554386884,
0.515848510308657));
#14428=CARTESIAN_POINT('Ctrl Pts',(-0.146424333269732,0.00801918670503405,
0.515631516033023));
#14429=CARTESIAN_POINT('Ctrl Pts',(-0.146099725131082,0.0119784074854107,
0.51541452175739));
#14430=CARTESIAN_POINT('Ctrl Pts',(-0.142141002193345,0.06026265009261,
0.512768191878288));
#14431=CARTESIAN_POINT('Ctrl Pts',(-0.111878319621163,0.106390286678145,
0.510121861999186));
#14432=CARTESIAN_POINT('Ctrl Pts',(-0.069163383343408,0.129247972261684,
0.507475532120084));
#14433=CARTESIAN_POINT('Ctrl Pts',(-0.0264484470656534,0.152105657845224,
0.504829202240982));
#14434=CARTESIAN_POINT('Ctrl Pts',(0.0287187429176733,0.151693392426768,
0.50218287236188));
#14435=CARTESIAN_POINT('Ctrl Pts',(0.07108729581893,0.128199876374419,0.499536542482778));
#14436=CARTESIAN_POINT('Ctrl Pts',(0.113455848720186,0.10470636032207,0.496890212603677));
#14437=CARTESIAN_POINT('Ctrl Pts',(0.143025764539373,0.0581315936358261,
0.494243882724575));
#14438=CARTESIAN_POINT('Ctrl Pts',(0.146262427589597,0.00979357977770552,
0.491597552845473));
#14439=CARTESIAN_POINT('Ctrl Pts',(0.149499090639821,-0.0385444340804161,
0.488951222966371));
#14440=CARTESIAN_POINT('Ctrl Pts',(0.126402500921083,-0.0886456951104151,
0.486304893087269));
#14441=CARTESIAN_POINT('Ctrl Pts',(0.087544330920799,-0.117578067907642,
0.483658563208167));
#14442=CARTESIAN_POINT('Ctrl Pts',(0.0486861609205161,-0.146510440704867,
0.481012233329065));
#14443=CARTESIAN_POINT('Ctrl Pts',(-0.00593358936131212,-0.154273925269321,
0.478365903449963));
#14444=CARTESIAN_POINT('Ctrl Pts',(-0.0513146009011563,-0.137315052574797,
0.475719573570861));
#14445=CARTESIAN_POINT('Ctrl Pts',(-0.0966956124410008,-0.120356179880273,
0.473073243691759));
#14446=CARTESIAN_POINT('Ctrl Pts',(-0.132837885238862,-0.078674949926771,
0.470426913812657));
#14447=CARTESIAN_POINT('Ctrl Pts',(-0.14319853241738,-0.0313495174248821,
0.467780583933555));
#14448=CARTESIAN_POINT('Ctrl Pts',(-0.145436768368387,-0.0211256884885646,
0.467208890817134));
#14449=CARTESIAN_POINT('Ctrl Pts',(-0.146471775395962,-0.0106384445195334,
0.466637197700712));
#14450=CARTESIAN_POINT('Ctrl Pts',(-0.146374718215768,-0.000132229735885947,
0.466065504584291));
#14451=CARTESIAN_POINT('Ctrl Pts',(-0.146375609273197,-0.000132432188538665,
0.458934495415711));
#14452=CARTESIAN_POINT('Ctrl Pts',(-0.146472577787773,-0.0106150565970108,
0.45950491398422));
#14453=CARTESIAN_POINT('Ctrl Pts',(-0.145442327125792,-0.021078770125739,
0.46007533255273));
#14454=CARTESIAN_POINT('Ctrl Pts',(-0.143213999951756,-0.0312807998000163,
0.460645751121239));
#14455=CARTESIAN_POINT('Ctrl Pts',(-0.132872033528166,-0.0786297930597184,
0.463293140495499));
#14456=CARTESIAN_POINT('Ctrl Pts',(-0.0967233424557573,-0.120342081894533,
0.465940529869759));
#14457=CARTESIAN_POINT('Ctrl Pts',(-0.0513258840937604,-0.13731129538499,
0.46858791924402));
#14458=CARTESIAN_POINT('Ctrl Pts',(-0.00592842573176499,-0.154280508875447,
0.47123530861828));
#14459=CARTESIAN_POINT('Ctrl Pts',(0.0487177999198187,-0.146506647021548,
0.47388269799254));
#14460=CARTESIAN_POINT('Ctrl Pts',(0.0875820145025328,-0.117550537871965,
0.476530087366799));
#14461=CARTESIAN_POINT('Ctrl Pts',(0.126446229085248,-0.0885944287223814,
0.47917747674106));
#14462=CARTESIAN_POINT('Ctrl Pts',(0.149528432599094,-0.0384560722771122,
0.481824866115319));
#14463=CARTESIAN_POINT('Ctrl Pts',(0.146255790172295,0.0098985887573764,
0.484472255489579));
#14464=CARTESIAN_POINT('Ctrl Pts',(0.142983147745498,0.0582532497918637,
0.487119644863839));
#14465=CARTESIAN_POINT('Ctrl Pts',(0.113355659378058,0.10482421541557,0.4897670342381));
#14466=CARTESIAN_POINT('Ctrl Pts',(0.0709442366160257,0.128279591164298,
0.49241442361236));
#14467=CARTESIAN_POINT('Ctrl Pts',(0.0285328138539934,0.151734966913027,
0.49506181298662));
#14468=CARTESIAN_POINT('Ctrl Pts',(-0.0266625433026316,0.152074752786777,
0.497709202360879));
#14469=CARTESIAN_POINT('Ctrl Pts',(-0.0693595260588707,0.129143309401606,
0.500356591735139));
#14470=CARTESIAN_POINT('Ctrl Pts',(-0.11205650881511,0.106211866016435,
0.503003981109399));
#14471=CARTESIAN_POINT('Ctrl Pts',(-0.142255117170964,0.060009193372344,
0.505651370483659));
#14472=CARTESIAN_POINT('Ctrl Pts',(-0.146122837288996,0.0116984888307781,
0.50829875985792));
#14473=CARTESIAN_POINT('Ctrl Pts',(-0.146432431239741,0.00783142983325791,
0.508510671710517));
#14474=CARTESIAN_POINT('Ctrl Pts',(-0.14657331536999,0.00395086404934249,
0.508722583563114));
#14475=CARTESIAN_POINT('Ctrl Pts',(-0.146550766805835,6.86360251013434E-5,
0.508934495415711));
#14476=CARTESIAN_POINT('Origin',(0.,0.,0.));
#14477=CARTESIAN_POINT('',(-0.146165204287215,8.83645032875094E-5,0.566065504584291));
#14478=CARTESIAN_POINT('',(-0.146168951232552,9.12430751481418E-5,0.558934495415711));
#14479=CARTESIAN_POINT('',(-0.14635,-1.79227059055215E-17,0.));
#14480=CARTESIAN_POINT('Ctrl Pts',(-0.146165204287215,8.83645032875094E-5,
0.566065504584291));
#14481=CARTESIAN_POINT('Ctrl Pts',(-0.146267412293664,0.0186373661349918,
0.565059822916602));
#14482=CARTESIAN_POINT('Ctrl Pts',(-0.142994166834961,0.0371516370495788,
0.564054141248913));
#14483=CARTESIAN_POINT('Ctrl Pts',(-0.136179985035193,0.0542551712289143,
0.563048459581224));
#14484=CARTESIAN_POINT('Ctrl Pts',(-0.118249288396568,0.0992610562830057,
0.560402129702122));
#14485=CARTESIAN_POINT('Ctrl Pts',(-0.0758005933416487,0.134498778989873,
0.55775579982302));
#14486=CARTESIAN_POINT('Ctrl Pts',(-0.0282633354322908,0.143839479279877,
0.555109469943918));
#14487=CARTESIAN_POINT('Ctrl Pts',(0.0192739224770691,0.153180179569881,
0.552463140064816));
#14488=CARTESIAN_POINT('Ctrl Pts',(0.0718997432408687,0.136623857443018,
0.549816810185715));
#14489=CARTESIAN_POINT('Ctrl Pts',(0.105526460745998,0.101748602013432,
0.547170480306613));
#14490=CARTESIAN_POINT('Ctrl Pts',(0.139153178251127,0.0668733465838454,
0.544524150427511));
#14491=CARTESIAN_POINT('Ctrl Pts',(0.153780792497586,0.0136791578515372,
0.541877820548409));
#14492=CARTESIAN_POINT('Ctrl Pts',(0.142714014311998,-0.0334861471092027,
0.539231490669307));
#14493=CARTESIAN_POINT('Ctrl Pts',(0.13164723612641,-0.0806514520699426,
0.536585160790205));
#14494=CARTESIAN_POINT('Ctrl Pts',(0.0948860655087725,-0.121787873259113,
0.533938830911103));
#14495=CARTESIAN_POINT('Ctrl Pts',(0.0492566686055307,-0.138066623508903,
0.531292501032001));
#14496=CARTESIAN_POINT('Ctrl Pts',(0.00362727170228945,-0.154345373758693,
0.528646171152899));
#14497=CARTESIAN_POINT('Ctrl Pts',(-0.050870351486557,-0.145766453069103,
0.525999841273797));
#14498=CARTESIAN_POINT('Ctrl Pts',(-0.089291781429334,-0.116256568409877,
0.523353511394695));
#14499=CARTESIAN_POINT('Ctrl Pts',(-0.124562723435938,-0.0891664410515947,
0.520924175791227));
#14500=CARTESIAN_POINT('Ctrl Pts',(-0.146285818313441,-0.0444372186796531,
0.518494840187759));
#14501=CARTESIAN_POINT('Ctrl Pts',(-0.146548608312775,6.99729089778146E-5,
0.516065504584291));
#14502=CARTESIAN_POINT('Ctrl Pts',(-0.146550766805835,6.86360251013434E-5,
0.508934495415711));
#14503=CARTESIAN_POINT('Ctrl Pts',(-0.146291618860727,-0.0445493453248537,
0.511369972937373));
#14504=CARTESIAN_POINT('Ctrl Pts',(-0.124445252016267,-0.0893868858389474,
0.513805450459036));
#14505=CARTESIAN_POINT('Ctrl Pts',(-0.0890226177929609,-0.116463349340462,
0.516240927980699));
#14506=CARTESIAN_POINT('Ctrl Pts',(-0.0505178462986829,-0.145895746531099,
0.518888317354959));
#14507=CARTESIAN_POINT('Ctrl Pts',(0.00402852857008221,-0.154341804473332,
0.52153570672922));
#14508=CARTESIAN_POINT('Ctrl Pts',(0.0496314652424392,-0.137932794781367,
0.52418309610348));
#14509=CARTESIAN_POINT('Ctrl Pts',(0.0952344019147948,-0.121523785089403,
0.52683048547774));
#14510=CARTESIAN_POINT('Ctrl Pts',(0.131893900390741,-0.0802597077632436,
0.529477874851999));
#14511=CARTESIAN_POINT('Ctrl Pts',(0.14281802728161,-0.0330416298281342,
0.532125264226259));
#14512=CARTESIAN_POINT('Ctrl Pts',(0.153742154172479,0.0141764481069759,
0.53477265360052));
#14513=CARTESIAN_POINT('Ctrl Pts',(0.138930909478268,0.0673485266510362,
0.53742004297478));
#14514=CARTESIAN_POINT('Ctrl Pts',(0.105168604077417,0.102119062543277,
0.54006743234904));
#14515=CARTESIAN_POINT('Ctrl Pts',(0.0714062986765666,0.136889598435517,
0.5427148217233));
#14516=CARTESIAN_POINT('Ctrl Pts',(0.018692932569077,0.153258591675938,
0.545362211097559));
#14517=CARTESIAN_POINT('Ctrl Pts',(-0.0288260648428939,0.143728202535144,
0.548009600471819));
#14518=CARTESIAN_POINT('Ctrl Pts',(-0.0763450622548654,0.13419781339435,
0.550656989846079));
#14519=CARTESIAN_POINT('Ctrl Pts',(-0.118669690971318,0.0987680418723385,
0.55330437922034));
#14520=CARTESIAN_POINT('Ctrl Pts',(-0.136413096952957,0.0536675432455532,
0.5559517685946));
#14521=CARTESIAN_POINT('Ctrl Pts',(-0.143076734904351,0.036729792140314,
0.556946010868304));
#14522=CARTESIAN_POINT('Ctrl Pts',(-0.146273385252938,0.0184280612467595,
0.557940253142007));
#14523=CARTESIAN_POINT('Ctrl Pts',(-0.146168951232552,9.12430751481418E-5,
0.558934495415711));
#14524=CARTESIAN_POINT('Origin',(0.,0.,0.));
#14525=CARTESIAN_POINT('',(-0.146227179098081,-0.000117664897458569,0.616065504584291));
#14526=CARTESIAN_POINT('',(-0.146218520919543,-0.000115076211918358,0.608934495415711));
#14527=CARTESIAN_POINT('',(-0.14635,-1.79227059055215E-17,0.));
#14528=CARTESIAN_POINT('Ctrl Pts',(-0.146227179098081,-0.000117664897458569,
0.616065504584291));
#14529=CARTESIAN_POINT('Ctrl Pts',(-0.145977603365176,0.0329427899635141,
0.614271135524546));
#14530=CARTESIAN_POINT('Ctrl Pts',(-0.134874795495675,0.0661550248562671,
0.612476766464802));
#14531=CARTESIAN_POINT('Ctrl Pts',(-0.114309815624116,0.091770790457776,
0.610682397405058));
#14532=CARTESIAN_POINT('Ctrl Pts',(-0.0839806476072558,0.129548841477563,
0.608036067525956));
#14533=CARTESIAN_POINT('Ctrl Pts',(-0.0330710111925292,0.150804375664025,
0.605389737646855));
#14534=CARTESIAN_POINT('Ctrl Pts',(0.0151169520838501,0.145808400611758,
0.602743407767753));
#14535=CARTESIAN_POINT('Ctrl Pts',(0.0633049153602295,0.140812425559491,
0.600097077888651));
#14536=CARTESIAN_POINT('Ctrl Pts',(0.108771205498262,0.109564941268491,
0.597450748009549));
#14537=CARTESIAN_POINT('Ctrl Pts',(0.130705186191441,0.0663684129079872,
0.594804418130447));
#14538=CARTESIAN_POINT('Ctrl Pts',(0.152639166884621,0.023171884547483,
0.592158088251345));
#14539=CARTESIAN_POINT('Ctrl Pts',(0.151040838132949,-0.0319736878825246,
0.589511758372243));
#14540=CARTESIAN_POINT('Ctrl Pts',(0.126641780152193,-0.0738273082886534,
0.586865428493141));
#14541=CARTESIAN_POINT('Ctrl Pts',(0.102242722171437,-0.115680928694782,
0.584219098614039));
#14542=CARTESIAN_POINT('Ctrl Pts',(0.0550429349615966,-0.14424259707703,
0.581572768734937));
#14543=CARTESIAN_POINT('Ctrl Pts',(0.00664650371163741,-0.14643918846291,
0.578926438855836));
#14544=CARTESIAN_POINT('Ctrl Pts',(-0.0417499275383225,-0.148635779848789,
0.576280108976733));
#14545=CARTESIAN_POINT('Ctrl Pts',(-0.0913430028284016,-0.1244672942383,
0.573633779097631));
#14546=CARTESIAN_POINT('Ctrl Pts',(-0.119433191362276,-0.0849960277323969,
0.570987449218529));
#14547=CARTESIAN_POINT('Ctrl Pts',(-0.136848298201485,-0.0605249807527623,
0.569346801007117));
#14548=CARTESIAN_POINT('Ctrl Pts',(-0.145998464265635,-0.0301720919893573,
0.567706152795704));
#14549=CARTESIAN_POINT('Ctrl Pts',(-0.146165204287215,8.83645032875094E-5,
0.566065504584291));
#14550=CARTESIAN_POINT('Ctrl Pts',(-0.146168951232552,9.12430751481418E-5,
0.558934495415711));
#14551=CARTESIAN_POINT('Ctrl Pts',(-0.145995306636495,-0.0303977620653178,
0.560587642516267));
#14552=CARTESIAN_POINT('Ctrl Pts',(-0.136695352934655,-0.0609837708898569,
0.562240789616823));
#14553=CARTESIAN_POINT('Ctrl Pts',(-0.119031718004195,-0.0855580991331628,
0.563893936717379));
#14554=CARTESIAN_POINT('Ctrl Pts',(-0.090744749826965,-0.124912017153538,
0.566541326091639));
#14555=CARTESIAN_POINT('Ctrl Pts',(-0.0410086302256792,-0.148848627462727,
0.5691887154659));
#14556=CARTESIAN_POINT('Ctrl Pts',(0.00739494322942312,-0.146403732988417,
0.57183610484016));
#14557=CARTESIAN_POINT('Ctrl Pts',(0.0557985166845234,-0.143958838514108,
0.57448349421442));
#14558=CARTESIAN_POINT('Ctrl Pts',(0.10286954399344,-0.1151324392563,0.57713088358868));
#14559=CARTESIAN_POINT('Ctrl Pts',(0.127047076753504,-0.0731285067993286,
0.579778272962939));
#14560=CARTESIAN_POINT('Ctrl Pts',(0.151224609513568,-0.031124574342357,
0.5824256623372));
#14561=CARTESIAN_POINT('Ctrl Pts',(0.15250864772478,0.0240568913137802,
0.58507305171146));
#14562=CARTESIAN_POINT('Ctrl Pts',(0.130311035929276,0.0671399443948921,
0.58772044108572));
#14563=CARTESIAN_POINT('Ctrl Pts',(0.108113424133771,0.110222997476006,
0.59036783045998));
#14564=CARTESIAN_POINT('Ctrl Pts',(0.0624341623315493,0.141207637982093,
0.593015219834239));
#14565=CARTESIAN_POINT('Ctrl Pts',(0.0141966988324609,0.145901308974836,
0.595662609208499));
#14566=CARTESIAN_POINT('Ctrl Pts',(-0.0340407646666261,0.150594979967579,
0.598309998582759));
#14567=CARTESIAN_POINT('Ctrl Pts',(-0.0848364298625779,0.128997681446978,
0.60095738795702));
#14568=CARTESIAN_POINT('Ctrl Pts',(-0.114923272877171,0.091002085522857,
0.60360477733128));
#14569=CARTESIAN_POINT('Ctrl Pts',(-0.135113526827902,0.0655045372973676,
0.60538135002609));
#14570=CARTESIAN_POINT('Ctrl Pts',(-0.14597798884013,0.0326223532682757,
0.6071579227209));
#14571=CARTESIAN_POINT('Ctrl Pts',(-0.146218520919543,-0.000115076211918358,
0.608934495415711));
#14572=CARTESIAN_POINT('Origin',(0.,0.,0.));
#14573=CARTESIAN_POINT('',(-0.146586033401767,-2.15382961294558E-5,0.66606550458429));
#14574=CARTESIAN_POINT('',(-0.146582846697157,-3.00215943766004E-5,0.65893449541571));
#14575=CARTESIAN_POINT('',(-0.14635,-1.79227059055215E-17,0.));
#14576=CARTESIAN_POINT('Ctrl Pts',(-0.146586033401767,-2.15382961294558E-5,
0.66606550458429));
#14577=CARTESIAN_POINT('Ctrl Pts',(-0.146488810225965,0.0472697707580183,
0.663482448132491));
#14578=CARTESIAN_POINT('Ctrl Pts',(-0.121516563758978,0.0946492637554097,
0.660899391680692));
#14579=CARTESIAN_POINT('Ctrl Pts',(-0.0824084263440199,0.121233094478226,
0.658316335228893));
#14580=CARTESIAN_POINT('Ctrl Pts',(-0.0423423130056393,0.148468111155377,
0.655670005349791));
#14581=CARTESIAN_POINT('Ctrl Pts',(0.0125607065496858,0.153876184485078,
0.653023675470689));
#14582=CARTESIAN_POINT('Ctrl Pts',(0.0571706564953393,0.134981954220393,
0.650377345591587));
#14583=CARTESIAN_POINT('Ctrl Pts',(0.101780606440992,0.116087723955709,
0.647731015712485));
#14584=CARTESIAN_POINT('Ctrl Pts',(0.136097486776972,0.0728911900966409,
0.645084685833384));
#14585=CARTESIAN_POINT('Ctrl Pts',(0.144413921474191,0.0251640857912735,
0.642438355954282));
#14586=CARTESIAN_POINT('Ctrl Pts',(0.152730356171409,-0.0225630185140953,
0.63979202607518));
#14587=CARTESIAN_POINT('Ctrl Pts',(0.135046345229863,-0.0748206932657649,
0.637145696196077));
#14588=CARTESIAN_POINT('Ctrl Pts',(0.0994561386758346,-0.10768977857233,
0.634499366316975));
#14589=CARTESIAN_POINT('Ctrl Pts',(0.0638659321218069,-0.140558863878895,
0.631853036437873));
#14590=CARTESIAN_POINT('Ctrl Pts',(0.0103695299552984,-0.154039359740357,
0.629206706558772));
#14591=CARTESIAN_POINT('Ctrl Pts',(-0.0365469229059137,-0.141961031115491,
0.62656037667967));
#14592=CARTESIAN_POINT('Ctrl Pts',(-0.0834633757671259,-0.129882702490626,
0.623914046800568));
#14593=CARTESIAN_POINT('Ctrl Pts',(-0.123799879323041,-0.0922455493794331,
0.621267716921466));
#14594=CARTESIAN_POINT('Ctrl Pts',(-0.139093781291504,-0.0462766888972804,
0.618621387042364));
#14595=CARTESIAN_POINT('Ctrl Pts',(-0.14401750805555,-0.0314774500153124,
0.617769426223006));
#14596=CARTESIAN_POINT('Ctrl Pts',(-0.14634567687575,-0.0158146654998378,
0.616917465403648));
#14597=CARTESIAN_POINT('Ctrl Pts',(-0.146227179098081,-0.000117664897458569,
0.616065504584291));
#14598=CARTESIAN_POINT('Ctrl Pts',(-0.146218520919543,-0.000115076211918358,
0.608934495415711));
#14599=CARTESIAN_POINT('Ctrl Pts',(-0.1463364217222,-0.0161618722236638,
0.60980531209516));
#14600=CARTESIAN_POINT('Ctrl Pts',(-0.143901781624712,-0.032173889023867,
0.61067612877461));
#14601=CARTESIAN_POINT('Ctrl Pts',(-0.138761720114909,-0.0472643972675185,
0.611546945454059));
#14602=CARTESIAN_POINT('Ctrl Pts',(-0.123135303504819,-0.0931413908061287,
0.614194334828319));
#14603=CARTESIAN_POINT('Ctrl Pts',(-0.0825044494514074,-0.130501484555709,
0.616841724202579));
#14604=CARTESIAN_POINT('Ctrl Pts',(-0.0354801761942514,-0.142231836504824,
0.619489113576839));
#14605=CARTESIAN_POINT('Ctrl Pts',(0.0115440970629072,-0.15396218845394,
0.6221365029511));
#14606=CARTESIAN_POINT('Ctrl Pts',(0.0649617895238099,-0.140062798602586,
0.624783892325359));
#14607=CARTESIAN_POINT('Ctrl Pts',(0.100304854137336,-0.106900301471969,
0.627431281699619));
#14608=CARTESIAN_POINT('Ctrl Pts',(0.135647918750861,-0.0737378043413545,
0.630078671073879));
#14609=CARTESIAN_POINT('Ctrl Pts',(0.15291635551701,-0.0213121999314781,
0.63272606044814));
#14610=CARTESIAN_POINT('Ctrl Pts',(0.144200333369931,0.026362891994447,
0.6353734498224));
#14611=CARTESIAN_POINT('Ctrl Pts',(0.135484311222852,0.0740379839203748,
0.63802083919666));
#14612=CARTESIAN_POINT('Ctrl Pts',(0.100783830162543,0.11696256336235,0.640668228570919));
#14613=CARTESIAN_POINT('Ctrl Pts',(0.055993492972559,0.135474968031154,
0.643315617945179));
#14614=CARTESIAN_POINT('Ctrl Pts',(0.0112031557825773,0.153987372699956,
0.64596300731944));
#14615=CARTESIAN_POINT('Ctrl Pts',(-0.04367703753708,0.148087602595587,
0.6486103966937));
#14616=CARTESIAN_POINT('Ctrl Pts',(-0.0835091394177698,0.120478055479053,
0.65125778606796));
#14617=CARTESIAN_POINT('Ctrl Pts',(-0.122009894390588,0.0937913289882395,
0.653816689183877));
#14618=CARTESIAN_POINT('Ctrl Pts',(-0.146451680634158,0.0468218259492564,
0.656375592299793));
#14619=CARTESIAN_POINT('Ctrl Pts',(-0.146582846697157,-3.00215943766004E-5,
0.65893449541571));
#14620=CARTESIAN_POINT('Origin',(0.,0.,0.));
#14621=CARTESIAN_POINT('',(-0.146290249280603,0.000131112932912382,0.716065504584291));
#14622=CARTESIAN_POINT('',(-0.146307221518699,0.000133045872591754,0.708934495415711));
#14623=CARTESIAN_POINT('',(-0.14635,-1.79227059055215E-17,0.));
#14624=CARTESIAN_POINT('Ctrl Pts',(-0.146290249280603,0.000131112932912382,
0.716065504584291));
#14625=CARTESIAN_POINT('Ctrl Pts',(-0.146406294125046,0.0134819654399978,
0.715340090619538));
#14626=CARTESIAN_POINT('Ctrl Pts',(-0.144729088574721,0.0268041890186768,
0.714614676654786));
#14627=CARTESIAN_POINT('Ctrl Pts',(-0.141142411757643,0.0395908011096033,
0.713889262690033));
#14628=CARTESIAN_POINT('Ctrl Pts',(-0.128058117149462,0.0862367098911347,
0.711242932810931));
#14629=CARTESIAN_POINT('Ctrl Pts',(-0.0895623832093418,0.125754646095387,
0.708596602931829));
#14630=CARTESIAN_POINT('Ctrl Pts',(-0.0432753130058998,0.140056628595385,
0.705950273052727));
#14631=CARTESIAN_POINT('Ctrl Pts',(0.00301175719754219,0.154358611095384,
0.703303943173625));
#14632=CARTESIAN_POINT('Ctrl Pts',(0.0570901636643063,0.143444639891129,
0.700657613294523));
#14633=CARTESIAN_POINT('Ctrl Pts',(0.0942073689518517,0.11231021130972,
0.698011283415421));
#14634=CARTESIAN_POINT('Ctrl Pts',(0.131324574239397,0.0811757827283121,
0.695364953536319));
#14635=CARTESIAN_POINT('Ctrl Pts',(0.151480578347723,0.0298208967697505,
0.692718623657217));
#14636=CARTESIAN_POINT('Ctrl Pts',(0.145449661086834,-0.0182485073085286,
0.690072293778115));
#14637=CARTESIAN_POINT('Ctrl Pts',(0.139418743825945,-0.0663179113868083,
0.687425963899014));
#14638=CARTESIAN_POINT('Ctrl Pts',(0.107200905195838,-0.111101833584806,
0.684779634019911));
#14639=CARTESIAN_POINT('Ctrl Pts',(0.0635427568131047,-0.132101968137704,
0.68213330414081));
#14640=CARTESIAN_POINT('Ctrl Pts',(0.0198846084303716,-0.153102102690602,
0.679486974261708));
#14641=CARTESIAN_POINT('Ctrl Pts',(-0.0352138497049885,-0.150318449598402,
0.676840644382606));
#14642=CARTESIAN_POINT('Ctrl Pts',(-0.0765331864534889,-0.125025130675956,
0.674194314503504));
#14643=CARTESIAN_POINT('Ctrl Pts',(-0.117852523201989,-0.0997318117535095,
0.671547984624402));
#14644=CARTESIAN_POINT('Ctrl Pts',(-0.14539273856363,-0.0519288270008166,
0.6689016547453));
#14645=CARTESIAN_POINT('Ctrl Pts',(-0.146548242683733,-0.00349635461217019,
0.666255324866198));
#14646=CARTESIAN_POINT('Ctrl Pts',(-0.146575870647472,-0.00233834005587287,
0.666192051438896));
#14647=CARTESIAN_POINT('Ctrl Pts',(-0.146588414938392,-0.00117996563262623,
0.666128778011593));
#14648=CARTESIAN_POINT('Ctrl Pts',(-0.146586033401767,-2.15382961294558E-5,
0.66606550458429));
#14649=CARTESIAN_POINT('Ctrl Pts',(-0.146582846697157,-3.00215943766004E-5,
0.65893449541571));
#14650=CARTESIAN_POINT('Ctrl Pts',(-0.146587382388275,-0.00165014728799839,
0.659022981674053));
#14651=CARTESIAN_POINT('Ctrl Pts',(-0.146562848415234,-0.00327013229389975,
0.659111467932396));
#14652=CARTESIAN_POINT('Ctrl Pts',(-0.146508820881567,-0.00488913307276392,
0.659199954190739));
#14653=CARTESIAN_POINT('Ctrl Pts',(-0.144892390022949,-0.0533274503793473,
0.661847343564999));
#14654=CARTESIAN_POINT('Ctrl Pts',(-0.116875517863988,-0.100884760863813,
0.66449473293926));
#14655=CARTESIAN_POINT('Ctrl Pts',(-0.0752913709948059,-0.125777373450206,
0.66714212231352));
#14656=CARTESIAN_POINT('Ctrl Pts',(-0.0337072241256252,-0.150669986036599,
0.66978951168778));
#14657=CARTESIAN_POINT('Ctrl Pts',(0.021444197453776,-0.15289790072492,
0.672436901062039));
#14658=CARTESIAN_POINT('Ctrl Pts',(0.0649007096996251,-0.131440618146733,
0.675084290436299));
#14659=CARTESIAN_POINT('Ctrl Pts',(0.108357221945475,-0.109983335568545,
0.677731679810559));
#14660=CARTESIAN_POINT('Ctrl Pts',(0.140118824857774,-0.0648408557238465,
0.68037906918482));
#14661=CARTESIAN_POINT('Ctrl Pts',(0.145637072805965,-0.0166907532130915,
0.68302645855908));
#14662=CARTESIAN_POINT('Ctrl Pts',(0.151155320754156,0.031459349297663,
0.68567384793334));
#14663=CARTESIAN_POINT('Ctrl Pts',(0.130430213738242,0.0826170744744734,
0.688321237307599));
#14664=CARTESIAN_POINT('Ctrl Pts',(0.0929549153570804,0.113349556369966,
0.690968626681859));
#14665=CARTESIAN_POINT('Ctrl Pts',(0.0554796169759186,0.14408203826546,
0.693616016056119));
#14666=CARTESIAN_POINT('Ctrl Pts',(0.00125412722950909,0.154389276879634,
0.69626340543038));
#14667=CARTESIAN_POINT('Ctrl Pts',(-0.0448834941801804,0.139550027475769,
0.69891079480464));
#14668=CARTESIAN_POINT('Ctrl Pts',(-0.0910211155898686,0.124710778071904,
0.7015581841789));
#14669=CARTESIAN_POINT('Ctrl Pts',(-0.129070868662838,0.0847250406500019,
0.704205573553159));
#14670=CARTESIAN_POINT('Ctrl Pts',(-0.141604011991841,0.0379083368947344,
0.706852962927419));
#14671=CARTESIAN_POINT('Ctrl Pts',(-0.144888775625201,0.0256383259412015,
0.707546807090183));
#14672=CARTESIAN_POINT('Ctrl Pts',(-0.146420824649375,0.0128991016161637,
0.708240651252947));
#14673=CARTESIAN_POINT('Ctrl Pts',(-0.146307221518699,0.000133045872591754,
0.708934495415711));
#14674=CARTESIAN_POINT('Origin',(0.,0.,0.));
#14675=CARTESIAN_POINT('',(-0.1461301977291,-5.61458017395017E-5,0.766065504584291));
#14676=CARTESIAN_POINT('',(-0.14612241379348,-4.54149644099216E-5,0.758934495415711));
#14677=CARTESIAN_POINT('',(-0.14635,-1.79227059055215E-17,0.));
#14678=CARTESIAN_POINT('Ctrl Pts',(-0.1461301977291,-5.61458017395017E-5,
0.766065504584291));
#14679=CARTESIAN_POINT('Ctrl Pts',(-0.14603380141711,0.0278870014676159,
0.764551403227483));
#14680=CARTESIAN_POINT('Ctrl Pts',(-0.138327245009168,0.0558793842949389,
0.763037301870675));
#14681=CARTESIAN_POINT('Ctrl Pts',(-0.123350675409043,0.079203679241543,
0.761523200513867));
#14682=CARTESIAN_POINT('Ctrl Pts',(-0.0971747899961838,0.119969628197767,
0.758876870634766));
#14683=CARTESIAN_POINT('Ctrl Pts',(-0.048790709571801,0.146475657227381,
0.756230540755664));
#14684=CARTESIAN_POINT('Ctrl Pts',(-0.000344588961360588,0.146589539830481,
0.753584210876561));
#14685=CARTESIAN_POINT('Ctrl Pts',(0.0481015316490792,0.14670342243358,
0.750937880997459));
#14686=CARTESIAN_POINT('Ctrl Pts',(0.0966096924455767,0.120425158610167,
0.748291551118357));
#14687=CARTESIAN_POINT('Ctrl Pts',(0.122976945064223,0.0797827231418903,
0.745645221239255));
#14688=CARTESIAN_POINT('Ctrl Pts',(0.149344197682869,0.0391402876736125,
0.742998891360154));
#14689=CARTESIAN_POINT('Ctrl Pts',(0.153570542123663,-0.01586631943953,
0.740352561481052));
#14690=CARTESIAN_POINT('Ctrl Pts',(0.133721514043982,-0.0600597087159893,
0.73770623160195));
#14691=CARTESIAN_POINT('Ctrl Pts',(0.113872485964301,-0.104253097992448,
0.735059901722848));
#14692=CARTESIAN_POINT('Ctrl Pts',(0.0699480853641458,-0.137633269432224,
0.732413571843746));
#14693=CARTESIAN_POINT('Ctrl Pts',(0.0220532014503509,-0.144921593405036,
0.729767241964644));
#14694=CARTESIAN_POINT('Ctrl Pts',(-0.0258416824634434,-0.152209917377848,
0.727120912085542));
#14695=CARTESIAN_POINT('Ctrl Pts',(-0.0777070496908773,-0.133406393883698,
0.724474582206441));
#14696=CARTESIAN_POINT('Ctrl Pts',(-0.109803305666473,-0.0971176914572187,
0.721828252327339));
#14697=CARTESIAN_POINT('Ctrl Pts',(-0.133101311474982,-0.0707764758164216,
0.71990733641299));
#14698=CARTESIAN_POINT('Ctrl Pts',(-0.14598295937539,-0.0352223077304616,
0.71798642049864));
#14699=CARTESIAN_POINT('Ctrl Pts',(-0.146290249280603,0.000131112932912382,
0.716065504584291));
#14700=CARTESIAN_POINT('Ctrl Pts',(-0.146307221518699,0.000133045872591754,
0.708934495415711));
#14701=CARTESIAN_POINT('Ctrl Pts',(-0.145987367488279,-0.0358102803178394,
0.710888040627207));
#14702=CARTESIAN_POINT('Ctrl Pts',(-0.132622002370819,-0.0719663061161047,
0.712841585838703));
#14703=CARTESIAN_POINT('Ctrl Pts',(-0.1086007072861,-0.0984612847532928,
0.7147951310502));
#14704=CARTESIAN_POINT('Ctrl Pts',(-0.0760477256663158,-0.134366532557423,
0.71744252042446));
#14705=CARTESIAN_POINT('Ctrl Pts',(-0.0239252288417074,-0.152529358077047,
0.720089909798719));
#14706=CARTESIAN_POINT('Ctrl Pts',(0.0238920022682765,-0.144630254255197,
0.722737299172979));
#14707=CARTESIAN_POINT('Ctrl Pts',(0.071709233378259,-0.136731150433346,
0.725384688547239));
#14708=CARTESIAN_POINT('Ctrl Pts',(0.115221198773618,-0.102770117270024,
0.7280320779215));
#14709=CARTESIAN_POINT('Ctrl Pts',(0.134497183226257,-0.058303052428779,
0.730679467295759));
#14710=CARTESIAN_POINT('Ctrl Pts',(0.153773167678896,-0.0138359875875333,
0.733326856670019));
#14711=CARTESIAN_POINT('Ctrl Pts',(0.148813171188813,0.0411371089316358,
0.735974246044279));
#14712=CARTESIAN_POINT('Ctrl Pts',(0.121889126928366,0.0814357351225549,
0.738621635418539));
#14713=CARTESIAN_POINT('Ctrl Pts',(0.0949650826679194,0.121734361313473,
0.741269024792799));
#14714=CARTESIAN_POINT('Ctrl Pts',(0.0460769906371109,0.147358517176143,
0.74391641416706));
#14715=CARTESIAN_POINT('Ctrl Pts',(-0.00238189178169058,0.146571023090686,
0.74656380354132));
#14716=CARTESIAN_POINT('Ctrl Pts',(-0.0508407742004934,0.14578352900523,
0.74921119291558));
#14717=CARTESIAN_POINT('Ctrl Pts',(-0.0988704470072894,0.118584384971644,
0.751858582289839));
#14718=CARTESIAN_POINT('Ctrl Pts',(-0.124470852918682,0.0774321960944291,
0.754505971664099));
#14719=CARTESIAN_POINT('Ctrl Pts',(-0.138745545153454,0.0544858868428234,
0.75598214624797));
#14720=CARTESIAN_POINT('Ctrl Pts',(-0.146046671909043,0.027201385339783,
0.757458320831841));
#14721=CARTESIAN_POINT('Ctrl Pts',(-0.14612241379348,-4.54149644099216E-5,
0.758934495415711));
#14722=CARTESIAN_POINT('Origin',(0.,0.,0.));
#14723=CARTESIAN_POINT('',(-0.146495788566881,-0.000101744904923998,0.816065504584291));
#14724=CARTESIAN_POINT('',(-0.146473871348434,-0.000110945968026819,0.808934495415711));
#14725=CARTESIAN_POINT('',(-0.14635,-1.79227059055215E-17,0.));
#14726=CARTESIAN_POINT('Ctrl Pts',(-0.146495788566881,-0.000101744904923998,
0.816065504584291));
#14727=CARTESIAN_POINT('Ctrl Pts',(-0.14616118452328,0.0421270051992108,
0.813762715835428));
#14728=CARTESIAN_POINT('Ctrl Pts',(-0.126905337350145,0.0846218946815527,
0.811459927086565));
#14729=CARTESIAN_POINT('Ctrl Pts',(-0.0947343415465314,0.111866064832055,
0.809157138337701));
#14730=CARTESIAN_POINT('Ctrl Pts',(-0.0577639214515077,0.143174651664521,
0.806510808458599));
#14731=CARTESIAN_POINT('Ctrl Pts',(-0.00373742343573488,0.154342745753647,
0.803864478579497));
#14732=CARTESIAN_POINT('Ctrl Pts',(0.0426163743729279,0.140258534729872,
0.801218148700395));
#14733=CARTESIAN_POINT('Ctrl Pts',(0.0889701721815907,0.126174323706097,
0.798571818821294));
#14734=CARTESIAN_POINT('Ctrl Pts',(0.127651269783143,0.0868378075694234,
0.795925488942192));
#14735=CARTESIAN_POINT('Ctrl Pts',(0.140954720244851,0.040253928627653,
0.79327915906309));
#14736=CARTESIAN_POINT('Ctrl Pts',(0.154258170706558,-0.00632995031411615,
0.790632829183988));
#14737=CARTESIAN_POINT('Ctrl Pts',(0.14218397402842,-0.060161192060982,
0.787986499304886));
#14738=CARTESIAN_POINT('Ctrl Pts',(0.110258679990485,-0.0966003903512828,
0.785340169425784));
#14739=CARTESIAN_POINT('Ctrl Pts',(0.0783333859525485,-0.133039588641585,
0.782693839546682));
#14740=CARTESIAN_POINT('Ctrl Pts',(0.0265569945548152,-0.152086743475322,
0.780047509667581));
#14741=CARTESIAN_POINT('Ctrl Pts',(-0.021371625274328,-0.14502367242074,
0.777401179788479));
#14742=CARTESIAN_POINT('Ctrl Pts',(-0.0693002451034712,-0.137960601366157,
0.774754849909377));
#14743=CARTESIAN_POINT('Ctrl Pts',(-0.113381093364023,-0.104787304423254,
0.772108520030274));
#14744=CARTESIAN_POINT('Ctrl Pts',(-0.133437672293631,-0.0606877215103841,
0.769462190151172));
#14745=CARTESIAN_POINT('Ctrl Pts',(-0.1420188514214,-0.0418197768941368,
0.768329961628878));
#14746=CARTESIAN_POINT('Ctrl Pts',(-0.146202281842484,-0.0209517273285418,
0.767197733106584));
#14747=CARTESIAN_POINT('Ctrl Pts',(-0.1461301977291,-5.61458017395017E-5,
0.766065504584291));
#14748=CARTESIAN_POINT('Ctrl Pts',(-0.14612241379348,-4.54149644099216E-5,
0.758934495415711));
#14749=CARTESIAN_POINT('Ctrl Pts',(-0.146182508321779,-0.0216633562673834,
0.760105710206101));
#14750=CARTESIAN_POINT('Ctrl Pts',(-0.141694203021096,-0.0432575645610501,
0.76127692499649));
#14751=CARTESIAN_POINT('Ctrl Pts',(-0.132531725405586,-0.0626424774360703,
0.76244813978688));
#14752=CARTESIAN_POINT('Ctrl Pts',(-0.111821052965107,-0.106459728368519,
0.76509552916114));
#14753=CARTESIAN_POINT('Ctrl Pts',(-0.067228569068158,-0.138988996512573,
0.767742918535399));
#14754=CARTESIAN_POINT('Ctrl Pts',(-0.0191799219195066,-0.145330206128911,
0.770390307909659));
#14755=CARTESIAN_POINT('Ctrl Pts',(0.0288687252291434,-0.151671415745249,
0.773037697283919));
#14756=CARTESIAN_POINT('Ctrl Pts',(0.080373535629496,-0.131824566833873,
0.77568508665818));
#14757=CARTESIAN_POINT('Ctrl Pts',(0.111742660473083,-0.0948805356683208,
0.77833247603244));
#14758=CARTESIAN_POINT('Ctrl Pts',(0.14311178531667,-0.0579365045027684,
0.7809798654067));
#14759=CARTESIAN_POINT('Ctrl Pts',(0.154345224603492,-0.00389529108304171,
0.783627254780959));
#14760=CARTESIAN_POINT('Ctrl Pts',(0.140297486112651,0.0424894529122293,
0.786274644155219));
#14761=CARTESIAN_POINT('Ctrl Pts',(0.126249747621811,0.0888741969075009,
0.788922033529479));
#14762=CARTESIAN_POINT('Ctrl Pts',(0.0869208313533056,0.127602471478316,
0.79156942290374));
#14763=CARTESIAN_POINT('Ctrl Pts',(0.0403254011646538,0.140934737517831,
0.794216812278));
#14764=CARTESIAN_POINT('Ctrl Pts',(-0.00627002902399674,0.154267003557346,
0.79686420165226));
#14765=CARTESIAN_POINT('Ctrl Pts',(-0.0601319731327944,0.142203261065564,
0.799511591026519));
#14766=CARTESIAN_POINT('Ctrl Pts',(-0.0965888940360299,0.110269323781398,
0.802158980400779));
#14767=CARTESIAN_POINT('Ctrl Pts',(-0.127690529151203,0.0830262752573849,
0.804417485405756));
#14768=CARTESIAN_POINT('Ctrl Pts',(-0.146124951115714,0.0413218847513699,
0.806675990410734));
#14769=CARTESIAN_POINT('Ctrl Pts',(-0.146473871348434,-0.000110945968026819,
0.808934495415711));
#14770=CARTESIAN_POINT('Origin',(0.,0.,0.));
#14771=CARTESIAN_POINT('',(-0.146444331750498,0.000119944961782359,0.866065504584291));
#14772=CARTESIAN_POINT('',(-0.146471560192382,0.00011177640072981,0.858934495415711));
#14773=CARTESIAN_POINT('',(-0.14635,-1.79227059055215E-17,0.));
#14774=CARTESIAN_POINT('Ctrl Pts',(-0.146444331750498,0.000119944961782359,
0.866065504584291));
#14775=CARTESIAN_POINT('Ctrl Pts',(-0.146516681599632,0.00829054204730037,
0.865620358322474));
#14776=CARTESIAN_POINT('Ctrl Pts',(-0.145891801779796,0.0164500693154795,
0.865175212060658));
#14777=CARTESIAN_POINT('Ctrl Pts',(-0.14453063157077,0.0244848619971339,
0.864730065798841));
#14778=CARTESIAN_POINT('Ctrl Pts',(-0.136438672357208,0.0722505376181754,
0.862083735919739));
#14779=CARTESIAN_POINT('Ctrl Pts',(-0.102325254887189,0.115607931012472,
0.859437406040638));
#14780=CARTESIAN_POINT('Ctrl Pts',(-0.0578046270350215,0.134711681091902,
0.856791076161536));
#14781=CARTESIAN_POINT('Ctrl Pts',(-0.0132839991828526,0.153815431171333,
0.854144746282434));
#14782=CARTESIAN_POINT('Ctrl Pts',(0.0416438390514653,0.148665537935894,
0.851498416403331));
#14783=CARTESIAN_POINT('Ctrl Pts',(0.081837551941475,0.121619188541491,
0.848852086524229));
#14784=CARTESIAN_POINT('Ctrl Pts',(0.122031264831484,0.0945728391470885,
0.846205756645128));
#14785=CARTESIAN_POINT('Ctrl Pts',(0.147490852377186,0.0456300335937214,
0.843559426766026));
#14786=CARTESIAN_POINT('Ctrl Pts',(0.146563060809277,-0.0028073360113171,
0.840913096886925));
#14787=CARTESIAN_POINT('Ctrl Pts',(0.145635269241369,-0.0512447056163556,
0.838266767007823));
#14788=CARTESIAN_POINT('Ctrl Pts',(0.118320098559852,-0.0991766392730661,
0.835620437128721));
#14789=CARTESIAN_POINT('Ctrl Pts',(0.0771201321287374,-0.124663936845065,
0.832974107249619));
#14790=CARTESIAN_POINT('Ctrl Pts',(0.035920165697623,-0.150151234417064,
0.830327777370517));
#14791=CARTESIAN_POINT('Ctrl Pts',(-0.0191645964830881,-0.153193895904352,
0.827681447491415));
#14792=CARTESIAN_POINT('Ctrl Pts',(-0.0629209921278279,-0.132399247274726,
0.825035117612313));
#14793=CARTESIAN_POINT('Ctrl Pts',(-0.106677387772568,-0.111604598645101,
0.822388787733211));
#14794=CARTESIAN_POINT('Ctrl Pts',(-0.139105416881337,-0.0669726398985626,
0.819742457854109));
#14795=CARTESIAN_POINT('Ctrl Pts',(-0.145362260348583,-0.0189321207373897,
0.817096127975007));
#14796=CARTESIAN_POINT('Ctrl Pts',(-0.146174510965348,-0.0126955988357878,
0.816752586844768));
#14797=CARTESIAN_POINT('Ctrl Pts',(-0.146545706411658,-0.00640163348415362,
0.81640904571453));
#14798=CARTESIAN_POINT('Ctrl Pts',(-0.146495788566881,-0.000101744904923998,
0.816065504584291));
#14799=CARTESIAN_POINT('Ctrl Pts',(-0.146473871348434,-0.000110945968026819,
0.808934495415711));
#14800=CARTESIAN_POINT('Ctrl Pts',(-0.146533950748007,-0.00724512552769256,
0.809323379784994));
#14801=CARTESIAN_POINT('Ctrl Pts',(-0.146057826922151,-0.0143712538186879,
0.809712264154277));
#14802=CARTESIAN_POINT('Ctrl Pts',(-0.145017839345608,-0.0214141189368497,
0.81010114852356));
#14803=CARTESIAN_POINT('Ctrl Pts',(-0.137937966054276,-0.0693594922943736,
0.81274853789782));
#14804=CARTESIAN_POINT('Ctrl Pts',(-0.104726321773939,-0.113446106932874,
0.81539592727208));
#14805=CARTESIAN_POINT('Ctrl Pts',(-0.0605955455659204,-0.133480028752914,
0.818043316646339));
#14806=CARTESIAN_POINT('Ctrl Pts',(-0.0164647693578984,-0.153513950572954,
0.820690706020599));
#14807=CARTESIAN_POINT('Ctrl Pts',(0.0385851387778066,-0.149495179574532,
0.823338095394859));
#14808=CARTESIAN_POINT('Ctrl Pts',(0.0793384931690736,-0.12326451930694,
0.825985484769119));
#14809=CARTESIAN_POINT('Ctrl Pts',(0.120091847560339,-0.0970338590393495,
0.828632874143379));
#14810=CARTESIAN_POINT('Ctrl Pts',(0.146548648207165,-0.0485913095025905,
0.83128026351764));
#14811=CARTESIAN_POINT('Ctrl Pts',(0.146590321408106,-0.000126046730599388,
0.833927652891899));
#14812=CARTESIAN_POINT('Ctrl Pts',(0.146631994609047,0.0483392160413931,
0.836575042266159));
#14813=CARTESIAN_POINT('Ctrl Pts',(0.120258540364101,0.0968271920486179,
0.839222431640419));
#14814=CARTESIAN_POINT('Ctrl Pts',(0.0795503554414038,0.123127897600245,
0.841869821014679));
#14815=CARTESIAN_POINT('Ctrl Pts',(0.0388421705187073,0.149428603151872,
0.844517210388939));
#14816=CARTESIAN_POINT('Ctrl Pts',(-0.0162007450817403,0.153542038247903,
0.8471645997632));
#14817=CARTESIAN_POINT('Ctrl Pts',(-0.0603659086281491,0.133584038319734,
0.84981198913746));
#14818=CARTESIAN_POINT('Ctrl Pts',(-0.104531072174558,0.113626038391565,
0.85245937851172));
#14819=CARTESIAN_POINT('Ctrl Pts',(-0.137818483666928,0.0695966034391962,
0.855106767885979));
#14820=CARTESIAN_POINT('Ctrl Pts',(-0.144980798768897,0.0216634763286692,
0.857754157260239));
#14821=CARTESIAN_POINT('Ctrl Pts',(-0.146045237806912,0.0145398171508471,
0.858147603312063));
#14822=CARTESIAN_POINT('Ctrl Pts',(-0.146532654486068,0.00732993751956911,
0.858541049363887));
#14823=CARTESIAN_POINT('Ctrl Pts',(-0.146471560192382,0.00011177640072981,
0.858934495415711));
#14824=CARTESIAN_POINT('Origin',(0.,0.,0.));
#14825=CARTESIAN_POINT('',(-0.146114231148477,2.69008449349656E-5,0.916065504584291));
#14826=CARTESIAN_POINT('',(-0.146121644853617,4.41067432152685E-5,0.908934495415711));
#14827=CARTESIAN_POINT('',(-0.14635,-1.79227059055215E-17,0.));
#14828=CARTESIAN_POINT('Ctrl Pts',(-0.146114231148477,2.69008449349656E-5,
0.916065504584291));
#14829=CARTESIAN_POINT('Ctrl Pts',(-0.146151635159142,0.0228038459942234,
0.914831670930419));
#14830=CARTESIAN_POINT('Ctrl Pts',(-0.141147538069067,0.0455652341090756,
0.913597837276548));
#14831=CARTESIAN_POINT('Ctrl Pts',(-0.131015765267123,0.0657531838068269,
0.912364003622676));
#14832=CARTESIAN_POINT('Ctrl Pts',(-0.109285110563454,0.109052354902802,
0.909717673743574));
#14833=CARTESIAN_POINT('Ctrl Pts',(-0.0639662294071284,0.140513248471977,
0.907071343864472));
#14834=CARTESIAN_POINT('Ctrl Pts',(-0.015802286694576,0.145735718560985,
0.90442501398537));
#14835=CARTESIAN_POINT('Ctrl Pts',(0.0323616560179757,0.150958188649994,
0.901778684106268));
#14836=CARTESIAN_POINT('Ctrl Pts',(0.0833706602867547,0.129942235258839,
0.899132354227166));
#14837=CARTESIAN_POINT('Ctrl Pts',(0.113877102345416,0.0923071908936453,
0.896486024348064));
#14838=CARTESIAN_POINT('Ctrl Pts',(0.144383544404078,0.0546721465284523,
0.893839694468962));
#14839=CARTESIAN_POINT('Ctrl Pts',(0.15438742425262,0.000418011189221586,
0.891193364589861));
#14840=CARTESIAN_POINT('Ctrl Pts',(0.139309808695705,-0.0456222438118789,
0.888547034710759));
#14841=CARTESIAN_POINT('Ctrl Pts',(0.124232193138789,-0.0916624988129813,
0.885900704831657));
#14842=CARTESIAN_POINT('Ctrl Pts',(0.0840730821764119,-0.129488873475953,
0.883254374952555));
#14843=CARTESIAN_POINT('Ctrl Pts',(0.0372139327097935,-0.141787641004198,
0.880608045073453));
#14844=CARTESIAN_POINT('Ctrl Pts',(-0.00964521675682358,-0.154086408532443,
0.877961715194351));
#14845=CARTESIAN_POINT('Ctrl Pts',(-0.0632044047276821,-0.140857568925962,
0.875315385315249));
#14846=CARTESIAN_POINT('Ctrl Pts',(-0.0989487482345592,-0.108156170198829,
0.872669055436147));
#14847=CARTESIAN_POINT('Ctrl Pts',(-0.128680439645858,-0.0809555616469925,
0.870467871818862));
#14848=CARTESIAN_POINT('Ctrl Pts',(-0.146086572253705,-0.0402824710322022,
0.868266688201576));
#14849=CARTESIAN_POINT('Ctrl Pts',(-0.146444331750498,0.000119944961782359,
0.866065504584291));
#14850=CARTESIAN_POINT('Ctrl Pts',(-0.146471560192382,0.00011177640072981,
0.858934495415711));
#14851=CARTESIAN_POINT('Ctrl Pts',(-0.146121567926216,-0.0412390669452651,
0.861188438738147));
#14852=CARTESIAN_POINT('Ctrl Pts',(-0.127770397964496,-0.0828616943330661,
0.863442382060584));
#14853=CARTESIAN_POINT('Ctrl Pts',(-0.096778382793969,-0.110103055552942,
0.86569632538302));
#14854=CARTESIAN_POINT('Ctrl Pts',(-0.0603764330055066,-0.142099641055337,
0.86834371475728));
#14855=CARTESIAN_POINT('Ctrl Pts',(-0.00653531471701479,-0.154255992791443,
0.870991104131539));
#14856=CARTESIAN_POINT('Ctrl Pts',(0.040082974241256,-0.14100387723139,
0.873638493505799));
#14857=CARTESIAN_POINT('Ctrl Pts',(0.0867012631995282,-0.127751761671338,
0.876285882880059));
#14858=CARTESIAN_POINT('Ctrl Pts',(0.12609672282758,-0.0890911788151255,
0.878933272254319));
#14859=CARTESIAN_POINT('Ctrl Pts',(0.140224208991091,-0.042730661487191,
0.88158066162858));
#14860=CARTESIAN_POINT('Ctrl Pts',(0.154351695154603,0.00362985584074295,
0.88422805100284));
#14861=CARTESIAN_POINT('Ctrl Pts',(0.143211207853577,0.057690307640398,
0.886875440377099));
#14862=CARTESIAN_POINT('Ctrl Pts',(0.111905662524754,0.09468823006692,0.889522829751359));
#14863=CARTESIAN_POINT('Ctrl Pts',(0.0806001171959318,0.131686152493442,
0.892170219125619));
#14864=CARTESIAN_POINT('Ctrl Pts',(0.0291295138393125,0.15162154554683,
0.894817608499879));
#14865=CARTESIAN_POINT('Ctrl Pts',(-0.0189299673197759,0.145362975188259,
0.897464997874139));
#14866=CARTESIAN_POINT('Ctrl Pts',(-0.0669894484788628,0.139104404829688,
0.9001123872484));
#14867=CARTESIAN_POINT('Ctrl Pts',(-0.11163780744042,0.10665187105916,0.902759776622659));
#14868=CARTESIAN_POINT('Ctrl Pts',(-0.132423802349956,0.0628703013313112,
0.905407165996919));
#14869=CARTESIAN_POINT('Ctrl Pts',(-0.141655418982822,0.043425734493323,
0.90658294246985));
#14870=CARTESIAN_POINT('Ctrl Pts',(-0.146180218154578,0.0217465313827003,
0.907758718942781));
#14871=CARTESIAN_POINT('Ctrl Pts',(-0.146121644853617,4.41067432152685E-5,
0.908934495415711));
#14872=CARTESIAN_POINT('Origin',(0.,0.,0.));
#14873=CARTESIAN_POINT('',(-0.146345621585321,-0.000133809880645736,0.966065504584291));
#14874=CARTESIAN_POINT('',(-0.146309694201085,-0.000133223314395004,0.958934495415711));
#14875=CARTESIAN_POINT('',(-0.14635,-1.79227059055215E-17,0.));
#14876=CARTESIAN_POINT('Ctrl Pts',(-0.146345621585321,-0.000133809880645736,
0.966065504584291));
#14877=CARTESIAN_POINT('Ctrl Pts',(-0.146004672532387,0.0370537288701324,
0.964042983538364));
#14878=CARTESIAN_POINT('Ctrl Pts',(-0.131578083002406,0.0744765756810296,
0.962020462492437));
#14879=CARTESIAN_POINT('Ctrl Pts',(-0.106003654037246,0.101251356830495,
0.959997941446511));
#14880=CARTESIAN_POINT('Ctrl Pts',(-0.0725412702228666,0.136284319036219,
0.957351611567409));
#14881=CARTESIAN_POINT('Ctrl Pts',(-0.0199938687303381,0.153087872523943,
0.954705281688306));
#14882=CARTESIAN_POINT('Ctrl Pts',(0.0275867780614433,0.143970766496025,
0.952058951809204));
#14883=CARTESIAN_POINT('Ctrl Pts',(0.0751674248532248,0.134853660468108,
0.949412621930102));
#14884=CARTESIAN_POINT('Ctrl Pts',(0.11778131694426,0.0998158949245492,
0.946766292051));
#14885=CARTESIAN_POINT('Ctrl Pts',(0.135923405490256,0.0548948063954655,
0.944119962171899));
#14886=CARTESIAN_POINT('Ctrl Pts',(0.154065494036253,0.0099737178663825,
0.941473632292797));
#14887=CARTESIAN_POINT('Ctrl Pts',(0.147735779037212,-0.0448306936482241,
0.938827302413695));
#14888=CARTESIAN_POINT('Ctrl Pts',(0.119831470632095,-0.0844335867733556,
0.936180972534593));
#14889=CARTESIAN_POINT('Ctrl Pts',(0.0919271622269763,-0.124036479898489,
0.933534642655491));
#14890=CARTESIAN_POINT('Ctrl Pts',(0.0424482604157787,-0.148437854634144,
0.93088831277639));
#14891=CARTESIAN_POINT('Ctrl Pts',(-0.00595796300272124,-0.146468817862788,
0.928241982897288));
#14892=CARTESIAN_POINT('Ctrl Pts',(-0.0543641864212212,-0.144499781091432,
0.925595653018186));
#14893=CARTESIAN_POINT('Ctrl Pts',(-0.101697731447024,-0.116160332813065,
0.922949323139084));
#14894=CARTESIAN_POINT('Ctrl Pts',(-0.126293289834417,-0.0744218843624929,
0.920302993259982));
#14895=CARTESIAN_POINT('Ctrl Pts',(-0.139421333187579,-0.052143709087005,
0.918890497034752));
#14896=CARTESIAN_POINT('Ctrl Pts',(-0.146071410932229,-0.0260482098028304,
0.917478000809521));
#14897=CARTESIAN_POINT('Ctrl Pts',(-0.146114231148477,2.69008449349656E-5,
0.916065504584291));
#14898=CARTESIAN_POINT('Ctrl Pts',(-0.146121644853617,4.41067432152685E-5,
0.908934495415711));
#14899=CARTESIAN_POINT('Ctrl Pts',(-0.146048333958771,-0.027118852224649,
0.910406108317041));
#14900=CARTESIAN_POINT('Ctrl Pts',(-0.138795050353101,-0.0543181883240968,
0.91187772121837));
#14901=CARTESIAN_POINT('Ctrl Pts',(-0.124603830013468,-0.0772180274565794,
0.9133493341197));
#14902=CARTESIAN_POINT('Ctrl Pts',(-0.0990742319099257,-0.118414180831446,
0.91599672349396));
#14903=CARTESIAN_POINT('Ctrl Pts',(-0.0510914048453256,-0.145695881896007,
0.91864411286822));
#14904=CARTESIAN_POINT('Ctrl Pts',(-0.00263394834681351,-0.146566710184873,
0.92129150224248));
#14905=CARTESIAN_POINT('Ctrl Pts',(0.0458235081516972,-0.147437538473739,
0.92393889161674));
#14906=CARTESIAN_POINT('Ctrl Pts',(0.0947555940841207,-0.121897493986912,
0.926586280990999));
#14907=CARTESIAN_POINT('Ctrl Pts',(0.121748900601314,-0.0816452290135895,
0.929233670365259));
#14908=CARTESIAN_POINT('Ctrl Pts',(0.148742207118509,-0.0413929640402651,
0.931881059739519));
#14909=CARTESIAN_POINT('Ctrl Pts',(0.153796734220472,0.0135715214195569,
0.93452844911378));
#14910=CARTESIAN_POINT('Ctrl Pts',(0.134597248858856,0.0580716696672091,
0.93717583848804));
#14911=CARTESIAN_POINT('Ctrl Pts',(0.115397763497239,0.102571817914861,
0.9398232278623));
#14912=CARTESIAN_POINT('Ctrl Pts',(0.0719442656720451,0.136607628950342,
0.942470617236559));
#14913=CARTESIAN_POINT('Ctrl Pts',(0.0241406894609324,0.144588953003544,
0.945118006610819));
#14914=CARTESIAN_POINT('Ctrl Pts',(-0.023662886750181,0.152570277056746,
0.947765395985079));
#14915=CARTESIAN_POINT('Ctrl Pts',(-0.0758165413472122,0.134497114127667,
0.950412785359339));
#14916=CARTESIAN_POINT('Ctrl Pts',(-0.108431221550465,0.0986479012011113,
0.953060174733599));
#14917=CARTESIAN_POINT('Ctrl Pts',(-0.132554242808212,0.0721325001574252,
0.955018281627637));
#14918=CARTESIAN_POINT('Ctrl Pts',(-0.145988218858404,0.0358924841874147,
0.956976388521674));
#14919=CARTESIAN_POINT('Ctrl Pts',(-0.146309694201085,-0.000133223314395004,
0.958934495415711));
#14920=CARTESIAN_POINT('Origin',(0.,0.,0.));
#14921=CARTESIAN_POINT('',(-0.146565171121453,5.44893591410845E-5,1.01606550458429));
#14922=CARTESIAN_POINT('',(-0.146582076026177,3.15354312248815E-5,1.00893449541571));
#14923=CARTESIAN_POINT('',(-0.14635,-1.79227059055215E-17,0.));
#14924=CARTESIAN_POINT('Ctrl Pts',(-0.146565171121453,5.44893591410845E-5,
1.01606550458429));
#14925=CARTESIAN_POINT('Ctrl Pts',(-0.146579596851449,0.00307427920823236,
1.01590062602541));
#14926=CARTESIAN_POINT('Ctrl Pts',(-0.146494352296349,0.00609323927190738,
1.01573574746653));
#14927=CARTESIAN_POINT('Ctrl Pts',(-0.146306854564556,0.00910583530985269,
1.01557086890765));
#14928=CARTESIAN_POINT('Ctrl Pts',(-0.143297482980539,0.0574585317612167,
1.01292453902855));
#14929=CARTESIAN_POINT('Ctrl Pts',(-0.11394685994478,0.104171803331984,
1.01027820914945));
#14930=CARTESIAN_POINT('Ctrl Pts',(-0.0716892273871119,0.127864250695428,
1.00763187927034));
#14931=CARTESIAN_POINT('Ctrl Pts',(-0.0294315948294418,0.151556698058874,
1.00498554939124));
#14932=CARTESIAN_POINT('Ctrl Pts',(0.0257330472501378,0.152228321214993,
1.00233921951214));
#14933=CARTESIAN_POINT('Ctrl Pts',(0.0685549742796134,0.129571707678744,
0.999692889633039));
#14934=CARTESIAN_POINT('Ctrl Pts',(0.111376901309088,0.106915094142495,
0.997046559753937));
#14935=CARTESIAN_POINT('Ctrl Pts',(0.141856113288459,0.0609302439138786,
0.994400229874835));
#14936=CARTESIAN_POINT('Ctrl Pts',(0.146041795372579,0.0126651464112397,
0.991753899995733));
#14937=CARTESIAN_POINT('Ctrl Pts',(0.150227477456699,-0.0355999510913994,
0.989107570116631));
#14938=CARTESIAN_POINT('Ctrl Pts',(0.128119629645567,-0.0861452958680607,
0.986461240237529));
#14939=CARTESIAN_POINT('Ctrl Pts',(0.0898373616998479,-0.115835488396583,
0.983814910358427));
#14940=CARTESIAN_POINT('Ctrl Pts',(0.051555093754129,-0.145525680925106,
0.981168580479325));
#14941=CARTESIAN_POINT('Ctrl Pts',(-0.00290159432617693,-0.154360721205491,
0.978522250600224));
#14942=CARTESIAN_POINT('Ctrl Pts',(-0.0486070196525971,-0.138296672301818,
0.975875920721122));
#14943=CARTESIAN_POINT('Ctrl Pts',(-0.0943124449790173,-0.122232623398145,
0.97322959084202));
#14944=CARTESIAN_POINT('Ctrl Pts',(-0.131266607551552,-0.081269485310415,
0.970583260962917));
#14945=CARTESIAN_POINT('Ctrl Pts',(-0.142555005769704,-0.0341567308046872,
0.967936931083816));
#14946=CARTESIAN_POINT('Ctrl Pts',(-0.145215975052668,-0.0230510282813687,
0.967313122250641));
#14947=CARTESIAN_POINT('Ctrl Pts',(-0.146450780951306,-0.0116036114945705,
0.966689313417466));
#14948=CARTESIAN_POINT('Ctrl Pts',(-0.146345621585321,-0.000133809880645736,
0.966065504584291));
#14949=CARTESIAN_POINT('Ctrl Pts',(-0.146309694201085,-0.000133223314395004,
0.958934495415711));
#14950=CARTESIAN_POINT('Ctrl Pts',(-0.146422858258782,-0.0128148032088542,
0.959623777895933));
#14951=CARTESIAN_POINT('Ctrl Pts',(-0.14491119500038,-0.0254698272036438,
0.960313060376156));
#14952=CARTESIAN_POINT('Ctrl Pts',(-0.141668994059001,-0.037664762585484,
0.961002342856379));
#14953=CARTESIAN_POINT('Ctrl Pts',(-0.129216380554811,-0.0845029505214961,
0.963649732230639));
#14954=CARTESIAN_POINT('Ctrl Pts',(-0.0912354477369537,-0.12455406346949,
0.966297121604899));
#14955=CARTESIAN_POINT('Ctrl Pts',(-0.0451234138007503,-0.1394726343957,
0.968944510979159));
#14956=CARTESIAN_POINT('Ctrl Pts',(0.00098862013545236,-0.154391205321909,
0.97159190035342));
#14957=CARTESIAN_POINT('Ctrl Pts',(0.055231755190001,-0.144177234226336,
0.974239289727679));
#14958=CARTESIAN_POINT('Ctrl Pts',(0.0927598492034174,-0.113509244531313,
0.976886679101939));
#14959=CARTESIAN_POINT('Ctrl Pts',(0.130287943216833,-0.0828412548362905,
0.979534068476199));
#14960=CARTESIAN_POINT('Ctrl Pts',(0.151100996189117,-0.0317192465418168,
0.982181457850459));
#14961=CARTESIAN_POINT('Ctrl Pts',(0.145665560755875,0.0164402745715088,
0.984828847224719));
#14962=CARTESIAN_POINT('Ctrl Pts',(0.140230125322634,0.0645997956848379,
0.987476236598979));
#14963=CARTESIAN_POINT('Ctrl Pts',(0.108546201483865,0.109796829617019,
0.990123625973239));
#14964=CARTESIAN_POINT('Ctrl Pts',(0.0651266538643092,0.131328813193254,
0.992771015347499));
#14965=CARTESIAN_POINT('Ctrl Pts',(0.0217071062447581,0.152860796769488,
0.995418404721759));
#14966=CARTESIAN_POINT('Ctrl Pts',(-0.0334480651555777,0.15072772998978,
0.998065794096019));
#14967=CARTESIAN_POINT('Ctrl Pts',(-0.0750749586823209,0.125906667008376,
1.00071318347028));
#14968=CARTESIAN_POINT('Ctrl Pts',(-0.116701852209067,0.101085604026969,
1.00336057284454));
#14969=CARTESIAN_POINT('Ctrl Pts',(-0.144800467862219,0.053576544843864,
1.0060079622188));
#14970=CARTESIAN_POINT('Ctrl Pts',(-0.146500196332402,0.00514107896046776,
1.00865535159306));
#14971=CARTESIAN_POINT('Ctrl Pts',(-0.146559936783033,0.00343871495990628,
1.00874839953394));
#14972=CARTESIAN_POINT('Ctrl Pts',(-0.146587066279139,0.00173520655478852,
1.00884144747483));
#14973=CARTESIAN_POINT('Ctrl Pts',(-0.146582076026177,3.15354312248815E-5,
1.00893449541571));
#14974=CARTESIAN_POINT('Origin',(0.,0.,0.));
#14975=CARTESIAN_POINT('',(-0.146184049129756,9.96948043307314E-5,1.06606550458429));
#14976=CARTESIAN_POINT('',(-0.146216477546812,0.000114345603752017,1.05893449541571));
#14977=CARTESIAN_POINT('',(-0.14635,-1.79227059055215E-17,0.));
#14978=CARTESIAN_POINT('Ctrl Pts',(-0.146184049129756,9.96948043307314E-5,
1.06606550458429));
#14979=CARTESIAN_POINT('Ctrl Pts',(-0.146294264763128,0.0176817746259609,
1.06511193863336));
#14980=CARTESIAN_POINT('Ctrl Pts',(-0.143360807533043,0.0352283113603788,
1.06415837268242));
#14981=CARTESIAN_POINT('Ctrl Pts',(-0.13721959397524,0.0515693218739058,
1.06320480673148));
#14982=CARTESIAN_POINT('Ctrl Pts',(-0.120176538991979,0.0969187854681546,
1.06055847685238));
#14983=CARTESIAN_POINT('Ctrl Pts',(-0.0784283132238915,0.132983650068601,
1.05791214697328));
#14984=CARTESIAN_POINT('Ctrl Pts',(-0.0310837364199337,0.143256459747686,
1.05526581709418));
#14985=CARTESIAN_POINT('Ctrl Pts',(0.0162608403840241,0.153529269426771,
1.05261948721508));
#14986=CARTESIAN_POINT('Ctrl Pts',(0.0692017682238519,0.138010024184496,
1.04997315733597));
#14987=CARTESIAN_POINT('Ctrl Pts',(0.103507151520239,0.103802126728842,
1.04732682745687));
#14988=CARTESIAN_POINT('Ctrl Pts',(0.137812534816628,0.0695942292731864,
1.04468049757777));
#14989=CARTESIAN_POINT('Ctrl Pts',(0.153482373569574,0.01669767960415,1.04203416769867));
#14990=CARTESIAN_POINT('Ctrl Pts',(0.143344336052008,-0.0306759392859165,
1.03938783781957));
#14991=CARTESIAN_POINT('Ctrl Pts',(0.133206298534443,-0.0780495581759789,
1.03674150794047));
#14992=CARTESIAN_POINT('Ctrl Pts',(0.0972603847463712,-0.119900246287072,
1.03409517806136));
#14993=CARTESIAN_POINT('Ctrl Pts',(0.0519596049571008,-0.137072285243832,
1.03144884818226));
#14994=CARTESIAN_POINT('Ctrl Pts',(0.00665882516783032,-0.154244324200591,
1.02880251830316));
#14995=CARTESIAN_POINT('Ctrl Pts',(-0.0479968206226384,-0.146737714003016,
1.02615618842406));
#14996=CARTESIAN_POINT('Ctrl Pts',(-0.0869905834517384,-0.11798834823825,
1.02350985854496));
#14997=CARTESIAN_POINT('Ctrl Pts',(-0.123554854979944,-0.0910302005802824,
1.02102840722473));
#14998=CARTESIAN_POINT('Ctrl Pts',(-0.146348061346918,-0.0453938791777224,
1.01854695590451));
#14999=CARTESIAN_POINT('Ctrl Pts',(-0.146565171121453,5.44893591410845E-5,
1.01606550458429));
#15000=CARTESIAN_POINT('Ctrl Pts',(-0.146582076026177,3.15354312248815E-5,
1.00893449541571));
#15001=CARTESIAN_POINT('Ctrl Pts',(-0.146445084172466,-0.0467374494427972,
1.01148883684909));
#15002=CARTESIAN_POINT('Ctrl Pts',(-0.122102455869861,-0.0936290599181376,
1.01404317828246));
#15003=CARTESIAN_POINT('Ctrl Pts',(-0.0837162036049941,-0.120334265578335,
1.01659751971584));
#15004=CARTESIAN_POINT('Ctrl Pts',(-0.0439316411201867,-0.14801227165006,
1.0192449090901));
#15005=CARTESIAN_POINT('Ctrl Pts',(0.0109383251366414,-0.154006411209824,
1.02189229846436));
#15006=CARTESIAN_POINT('Ctrl Pts',(0.0557604321169594,-0.135571060438576,
1.02453968783862));
#15007=CARTESIAN_POINT('Ctrl Pts',(0.100582539097277,-0.11713570966733,
1.02718707721288));
#15008=CARTESIAN_POINT('Ctrl Pts',(0.135356786801084,-0.0742708685650716,
1.02983446658714));
#15009=CARTESIAN_POINT('Ctrl Pts',(0.144154783532934,-0.0266108361928598,
1.0324818559614));
#15010=CARTESIAN_POINT('Ctrl Pts',(0.152952780264784,0.0210491961793507,
1.03512924533566));
#15011=CARTESIAN_POINT('Ctrl Pts',(0.135774526024679,0.0735044198215165,
1.03777663470992));
#15012=CARTESIAN_POINT('Ctrl Pts',(0.100488543649143,0.106727647840587,
1.04042402408418));
#15013=CARTESIAN_POINT('Ctrl Pts',(0.0652025612736062,0.139950875859659,
1.04307141345844));
#15014=CARTESIAN_POINT('Ctrl Pts',(0.0118088507626404,0.153942108255635,
1.0457188028327));
#15015=CARTESIAN_POINT('Ctrl Pts',(-0.0352355257975899,0.142292641904202,
1.04836619220696));
#15016=CARTESIAN_POINT('Ctrl Pts',(-0.0822799023578202,0.130643175552769,
1.05101358158122));
#15017=CARTESIAN_POINT('Ctrl Pts',(-0.122974944967313,0.0933530104539243,
1.05366097095548));
#15018=CARTESIAN_POINT('Ctrl Pts',(-0.138680233730631,0.0475029577050484,
1.05630836032974));
#15019=CARTESIAN_POINT('Ctrl Pts',(-0.143873300563147,0.0323423075707214,
1.05718373869173));
#15020=CARTESIAN_POINT('Ctrl Pts',(-0.146334133026589,0.0162457690968458,
1.05805911705372));
#15021=CARTESIAN_POINT('Ctrl Pts',(-0.146216477546812,0.000114345603752017,
1.05893449541571));
#15022=CARTESIAN_POINT('Origin',(0.,0.,0.));
#15023=CARTESIAN_POINT('',(-0.146204073634541,-0.000109175101205505,1.11606550458429));
#15024=CARTESIAN_POINT('',(-0.146170555016798,-9.22629125885076E-5,1.10893449541571));
#15025=CARTESIAN_POINT('',(-0.14635,-1.79227059055215E-17,0.));
#15026=CARTESIAN_POINT('Ctrl Pts',(-0.146204073634541,-0.000109175101205505,
1.11606550458429));
#15027=CARTESIAN_POINT('Ctrl Pts',(-0.145981599624502,0.032003853555373,
1.1143232512413));
#15028=CARTESIAN_POINT('Ctrl Pts',(-0.135565881201595,0.0642480963468658,
1.11258099789831));
#15029=CARTESIAN_POINT('Ctrl Pts',(-0.11609067353381,0.0895073597405865,
1.11083874455532));
#15030=CARTESIAN_POINT('Ctrl Pts',(-0.0865095427755784,0.127873963375947,
1.10819241467622));
#15031=CARTESIAN_POINT('Ctrl Pts',(-0.0360273159486943,0.150125560802435,
1.10554608479712));
#15032=CARTESIAN_POINT('Ctrl Pts',(0.0122494975033169,0.14607724579886,
1.10289975491801));
#15033=CARTESIAN_POINT('Ctrl Pts',(0.0605263109553308,0.142028930795284,
1.10025342503891));
#15034=CARTESIAN_POINT('Ctrl Pts',(0.10659771103247,0.111680703361642,1.09760709515981));
#15035=CARTESIAN_POINT('Ctrl Pts',(0.129376093089052,0.0689234246557527,
1.09496076528071));
#15036=CARTESIAN_POINT('Ctrl Pts',(0.152154475145634,0.0261661459498645,
1.09231443540161));
#15037=CARTESIAN_POINT('Ctrl Pts',(0.151639839181659,-0.0290001840282729,
1.0896681055225));
#15038=CARTESIAN_POINT('Ctrl Pts',(0.128067742174483,-0.0713250681289163,
1.0870217756434));
#15039=CARTESIAN_POINT('Ctrl Pts',(0.104495645167307,-0.11364995222956,
1.0843754457643));
#15040=CARTESIAN_POINT('Ctrl Pts',(0.0578660871169326,-0.143133390452712,
1.0817291158852));
#15041=CARTESIAN_POINT('Ctrl Pts',(0.00952215035475689,-0.146280349267719,
1.0790827860061));
#15042=CARTESIAN_POINT('Ctrl Pts',(-0.0388217864074202,-0.149427308082725,
1.07643645612699));
#15043=CARTESIAN_POINT('Ctrl Pts',(-0.0888801018813974,-0.126237787489585,
1.07379012624789));
#15044=CARTESIAN_POINT('Ctrl Pts',(-0.117740317519168,-0.0873259958989869,
1.07114379636879));
#15045=CARTESIAN_POINT('Ctrl Pts',(-0.136201180005177,-0.0624354946409797,
1.06945103244062));
#15046=CARTESIAN_POINT('Ctrl Pts',(-0.145988395071105,-0.0311118962502767,
1.06775826851246));
#15047=CARTESIAN_POINT('Ctrl Pts',(-0.146184049129756,9.96948043307314E-5,
1.06606550458429));
#15048=CARTESIAN_POINT('Ctrl Pts',(-0.146216477546812,0.000114345603752017,
1.05893449541571));
#15049=CARTESIAN_POINT('Ctrl Pts',(-0.145978309898544,-0.0325401742182177,
1.06070650642798));
#15050=CARTESIAN_POINT('Ctrl Pts',(-0.135174246449945,-0.06533764273189,
1.06247851744025));
#15051=CARTESIAN_POINT('Ctrl Pts',(-0.115079600404687,-0.0908043159161929,
1.06425052845252));
#15052=CARTESIAN_POINT('Ctrl Pts',(-0.0850581433982766,-0.128851596389654,
1.06689791782678));
#15053=CARTESIAN_POINT('Ctrl Pts',(-0.0342996944683099,-0.150536216937668,
1.06954530720104));
#15054=CARTESIAN_POINT('Ctrl Pts',(0.0139457694684962,-0.145925507476389,
1.0721926965753));
#15055=CARTESIAN_POINT('Ctrl Pts',(0.0621912334052997,-0.14131479801511,
1.07484008594956));
#15056=CARTESIAN_POINT('Ctrl Pts',(0.107923712348941,-0.110408758544542,
1.07748747532382));
#15057=CARTESIAN_POINT('Ctrl Pts',(0.1301953818052,-0.0673639426912374,
1.08013486469808));
#15058=CARTESIAN_POINT('Ctrl Pts',(0.15246705126146,-0.024319126837932,
1.08278225407234));
#15059=CARTESIAN_POINT('Ctrl Pts',(0.151277911230334,0.0308644653981125,
1.0854296434466));
#15060=CARTESIAN_POINT('Ctrl Pts',(0.127172648928576,0.0729099141598672,
1.08807703282086));
#15061=CARTESIAN_POINT('Ctrl Pts',(0.103067386626818,0.114955362921624,
1.09072442219512));
#15062=CARTESIAN_POINT('Ctrl Pts',(0.0560460020544268,0.143862668209093,
1.09337181156938));
#15063=CARTESIAN_POINT('Ctrl Pts',(0.00764670469074742,0.146390799320458,
1.09601920094364));
#15064=CARTESIAN_POINT('Ctrl Pts',(-0.0407525926729279,0.148918930431823,
1.0986665903179));
#15065=CARTESIAN_POINT('Ctrl Pts',(-0.0905298028278899,0.125067887367091,
1.10131397969216));
#15066=CARTESIAN_POINT('Ctrl Pts',(-0.11888440661962,0.0857626730052823,
1.10396136906642));
#15067=CARTESIAN_POINT('Ctrl Pts',(-0.136639133674055,0.0611510311732957,
1.10561907784952));
#15068=CARTESIAN_POINT('Ctrl Pts',(-0.145994366384503,0.0304800321277272,
1.10727678663261));
#15069=CARTESIAN_POINT('Ctrl Pts',(-0.146170555016798,-9.22629125885076E-5,
1.10893449541571));
#15070=CARTESIAN_POINT('Origin',(0.,0.,0.));
#15071=CARTESIAN_POINT('',(-0.146577386142569,-3.88073511912723E-5,1.16606550458429));
#15072=CARTESIAN_POINT('',(-0.146552328192774,-6.73160170860698E-5,1.15893449541571));
#15073=CARTESIAN_POINT('',(-0.14635,-1.79227059055215E-17,0.));
#15074=CARTESIAN_POINT('Ctrl Pts',(-0.146577386142569,-3.88073511912723E-5,
1.16606550458429));
#15075=CARTESIAN_POINT('Ctrl Pts',(-0.146413350709018,0.0463056768050285,
1.16353456384924));
#15076=CARTESIAN_POINT('Ctrl Pts',(-0.122574225104448,0.0927954474992645,
1.1610036231142));
#15077=CARTESIAN_POINT('Ctrl Pts',(-0.0847742546295189,0.119590709008994,
1.15847268237915));
#15078=CARTESIAN_POINT('Ctrl Pts',(-0.0452509303920754,0.147607604138013,
1.15582635250005));
#15079=CARTESIAN_POINT('Ctrl Pts',(0.00953524646069181,0.154093252855687,
1.15318002262095));
#15080=CARTESIAN_POINT('Ctrl Pts',(0.0545077808453859,0.136079071706768,
1.15053369274185));
#15081=CARTESIAN_POINT('Ctrl Pts',(0.0994803152300801,0.118064890557849,
1.14788736286275));
#15082=CARTESIAN_POINT('Ctrl Pts',(0.134639207146701,0.0755508795423365,
1.14524103298364));
#15083=CARTESIAN_POINT('Ctrl Pts',(0.14389167861853,0.027996370364851,1.14259470310454));
#15084=CARTESIAN_POINT('Ctrl Pts',(0.15314415009036,-0.0195581388126345,
1.13994837322544));
#15085=CARTESIAN_POINT('Ctrl Pts',(0.136490201117397,-0.0721531461520931,
1.13730204334634));
#15086=CARTESIAN_POINT('Ctrl Pts',(0.101552606157185,-0.105715089329518,
1.13465571346724));
#15087=CARTESIAN_POINT('Ctrl Pts',(0.0666150111969725,-0.139277032506943,
1.13200938358813));
#15088=CARTESIAN_POINT('Ctrl Pts',(0.0133937702495101,-0.153805911522335,
1.12936305370903));
#15089=CARTESIAN_POINT('Ctrl Pts',(-0.033750917386428,-0.142651629870951,
1.12671672382993));
#15090=CARTESIAN_POINT('Ctrl Pts',(-0.0808956050223675,-0.131497348219567,
1.12407039395083));
#15091=CARTESIAN_POINT('Ctrl Pts',(-0.121963739346782,-0.094659905901407,
1.12142406407173));
#15092=CARTESIAN_POINT('Ctrl Pts',(-0.1381577891642,-0.0490003798202082,
1.11877773419262));
#15093=CARTESIAN_POINT('Ctrl Pts',(-0.143690228857438,-0.0334015285560649,
1.11787365765651));
#15094=CARTESIAN_POINT('Ctrl Pts',(-0.146319518115206,-0.0167730178360648,
1.1169695811204));
#15095=CARTESIAN_POINT('Ctrl Pts',(-0.146204073634541,-0.000109175101205505,
1.11606550458429));
#15096=CARTESIAN_POINT('Ctrl Pts',(-0.146170555016798,-9.22629125885076E-5,
1.10893449541571));
#15097=CARTESIAN_POINT('Ctrl Pts',(-0.146275742653821,-0.0183444476975235,
1.10992417600687));
#15098=CARTESIAN_POINT('Ctrl Pts',(-0.143109248288425,-0.0365614514641733,
1.11091385659804));
#15099=CARTESIAN_POINT('Ctrl Pts',(-0.136505188007283,-0.0534328725168923,
1.1119035371892));
#15100=CARTESIAN_POINT('Ctrl Pts',(-0.118839368174718,-0.0985638180183679,
1.11455092656346));
#15101=CARTESIAN_POINT('Ctrl Pts',(-0.0765757310810901,-0.134066323362434,
1.11719831593772));
#15102=CARTESIAN_POINT('Ctrl Pts',(-0.0290731934694857,-0.143678417446031,
1.11984570531198));
#15103=CARTESIAN_POINT('Ctrl Pts',(0.01842934414212,-0.153290511529629,
1.12249309468624));
#15104=CARTESIAN_POINT('Ctrl Pts',(0.071170782271703,-0.137012194352758,
1.1251404840605));
#15105=CARTESIAN_POINT('Ctrl Pts',(0.10499283308901,-0.102299771349957,
1.12778787343476));
#15106=CARTESIAN_POINT('Ctrl Pts',(0.138814883906317,-0.0675873483471558,
1.13043526280902));
#15107=CARTESIAN_POINT('Ctrl Pts',(0.153717547411349,-0.0144408195184256,
1.13308265218328));
#15108=CARTESIAN_POINT('Ctrl Pts',(0.142874638214406,0.0327959749574983,
1.13573004155754));
#15109=CARTESIAN_POINT('Ctrl Pts',(0.132031729017462,0.0800327694334235,
1.1383774309318));
#15110=CARTESIAN_POINT('Ctrl Pts',(0.0954432471185425,0.121359829556542,
1.14102482030606));
#15111=CARTESIAN_POINT('Ctrl Pts',(0.0498685966661331,0.137847238945365,
1.14367220968032));
#15112=CARTESIAN_POINT('Ctrl Pts',(0.00429394621372511,0.154334648334189,
1.14631959905458));
#15113=CARTESIAN_POINT('Ctrl Pts',(-0.0502668727921719,0.145982406988718,
1.14896698842884));
#15114=CARTESIAN_POINT('Ctrl Pts',(-0.0888222026239048,0.116616270474356,
1.1516143778031));
#15115=CARTESIAN_POINT('Ctrl Pts',(-0.124357782404925,0.0895501633622979,
1.1540544170073));
#15116=CARTESIAN_POINT('Ctrl Pts',(-0.146296868742479,0.0446329749882746,
1.15649445621151));
#15117=CARTESIAN_POINT('Ctrl Pts',(-0.146552328192774,-6.73160170860698E-5,
1.15893449541571));
#15118=CARTESIAN_POINT('Origin',(0.,0.,0.));
#15119=CARTESIAN_POINT('',(-0.146318311025392,0.000133437649768732,1.21606550458429));
#15120=CARTESIAN_POINT('',(-0.146373054956946,0.000132657382717961,1.20893449541571));
#15121=CARTESIAN_POINT('',(-0.14635,-1.79227059055215E-17,0.));
#15122=CARTESIAN_POINT('Ctrl Pts',(-0.146318311025392,0.000133437649768732,
1.21606550458429));
#15123=CARTESIAN_POINT('Ctrl Pts',(-0.146429658069886,0.0125190846592594,
1.21539220633629));
#15124=CARTESIAN_POINT('Ctrl Pts',(-0.144988168643405,0.0248791929292086,
1.21471890808829));
#15125=CARTESIAN_POINT('Ctrl Pts',(-0.141892968227885,0.0368102906365087,
1.21404560984029));
#15126=CARTESIAN_POINT('Ctrl Pts',(-0.129727599662405,0.083704249513052,
1.21139927996119));
#15127=CARTESIAN_POINT('Ctrl Pts',(-0.0920156607298113,0.123970842060419,
1.20875295008209));
#15128=CARTESIAN_POINT('Ctrl Pts',(-0.0460184991925076,0.139179415364965,
1.20610662020299));
#15129=CARTESIAN_POINT('Ctrl Pts',(-2.13376552038805E-5,0.15438798866951,
1.20346029032389));
#15130=CARTESIAN_POINT('Ctrl Pts',(0.0542610464868107,0.144538542731236,
1.20081396044478));
#15131=CARTESIAN_POINT('Ctrl Pts',(0.091982751999895,0.114139323915075,
1.19816763056568));
#15132=CARTESIAN_POINT('Ctrl Pts',(0.129704457512977,0.0837401050989159,
1.19552130068658));
#15133=CARTESIAN_POINT('Ctrl Pts',(0.150865484397133,0.0327911134048729,
1.19287497080748));
#15134=CARTESIAN_POINT('Ctrl Pts',(0.145780097726084,-0.0153874961003253,
1.19022864092838));
#15135=CARTESIAN_POINT('Ctrl Pts',(0.140694711055036,-0.063566105605525,
1.18758231104927));
#15136=CARTESIAN_POINT('Ctrl Pts',(0.109362910828785,-0.108974332921877,
1.18493598117017));
#15137=CARTESIAN_POINT('Ctrl Pts',(0.0661257549466402,-0.130828118009858,
1.18228965129107));
#15138=CARTESIAN_POINT('Ctrl Pts',(0.0228885990644955,-0.152681903097838,
1.17964332141197));
#15139=CARTESIAN_POINT('Ctrl Pts',(-0.0322539124735426,-0.150981245957443,
1.17699699153287));
#15140=CARTESIAN_POINT('Ctrl Pts',(-0.0740621845924981,-0.126504564117865,
1.17435066165376));
#15141=CARTESIAN_POINT('Ctrl Pts',(-0.115870456711455,-0.102027882278287,
1.17170433177466));
#15142=CARTESIAN_POINT('Ctrl Pts',(-0.144344489411329,-0.0547751757395235,
1.16905800189556));
#15143=CARTESIAN_POINT('Ctrl Pts',(-0.146451269950206,-0.00637475169995868,
1.16641167201646));
#15144=CARTESIAN_POINT('Ctrl Pts',(-0.146543132875163,-0.00426432565444621,
1.1662962828724));
#15145=CARTESIAN_POINT('Ctrl Pts',(-0.146584864748453,-0.00215171749738942,
1.16618089372835));
#15146=CARTESIAN_POINT('Ctrl Pts',(-0.146577386142569,-3.88073511912723E-5,
1.16606550458429));
#15147=CARTESIAN_POINT('Ctrl Pts',(-0.146552328192774,-6.73160170860698E-5,
1.15893449541571));
#15148=CARTESIAN_POINT('Ctrl Pts',(-0.146574036680232,-0.00386586684592084,
1.15914184558577));
#15149=CARTESIAN_POINT('Ctrl Pts',(-0.1464391612665,-0.00766285139452399,
1.15934919575582));
#15150=CARTESIAN_POINT('Ctrl Pts',(-0.146142739258869,-0.0114471821958193,
1.15955654592588));
#15151=CARTESIAN_POINT('Ctrl Pts',(-0.142358105404532,-0.0597644666683822,
1.16220393530014));
#15152=CARTESIAN_POINT('Ctrl Pts',(-0.112238997038288,-0.106019003930254,
1.1648513246744));
#15153=CARTESIAN_POINT('Ctrl Pts',(-0.0695815129186611,-0.129023839960917,
1.16749871404866));
#15154=CARTESIAN_POINT('Ctrl Pts',(-0.026924028799035,-0.15202867599158,
1.17014610342292));
#15155=CARTESIAN_POINT('Ctrl Pts',(0.0282718310739737,-0.151783810791035,
1.17279349279718));
#15156=CARTESIAN_POINT('Ctrl Pts',(0.0707235276354612,-0.128401405199111,
1.17544088217144));
#15157=CARTESIAN_POINT('Ctrl Pts',(0.11317522419695,-0.105018999607187,
1.1780882715457));
#15158=CARTESIAN_POINT('Ctrl Pts',(0.142882757446916,-0.0584990536238821,
1.18073566091996));
#15159=CARTESIAN_POINT('Ctrl Pts',(0.146238551171451,-0.0101500920973681,
1.18338305029422));
#15160=CARTESIAN_POINT('Ctrl Pts',(0.149594344895986,0.0381988694291446,
1.18603043966848));
#15161=CARTESIAN_POINT('Ctrl Pts',(0.12659839909509,0.0883768464988665,
1.18867782904274));
#15162=CARTESIAN_POINT('Ctrl Pts',(0.0877840381772113,0.117399748124142,
1.191325218417));
#15163=CARTESIAN_POINT('Ctrl Pts',(0.0489696772593311,0.146422649749419,
1.19397260779126));
#15164=CARTESIAN_POINT('Ctrl Pts',(-0.00566309877553352,0.154290475930249,
1.19661999716552));
#15165=CARTESIAN_POINT('Ctrl Pts',(-0.0510896721842483,0.137399358129564,
1.19926738653978));
#15166=CARTESIAN_POINT('Ctrl Pts',(-0.0965162455929618,0.12050824032888,
1.20191477591404));
#15167=CARTESIAN_POINT('Ctrl Pts',(-0.132736616375526,0.0788581785466829,
1.2045621652883));
#15168=CARTESIAN_POINT('Ctrl Pts',(-0.143159994183491,0.0315270405159292,
1.20720955466256));
#15169=CARTESIAN_POINT('Ctrl Pts',(-0.145423823013163,0.021247302336111,
1.20778453491361));
#15170=CARTESIAN_POINT('Ctrl Pts',(-0.146470795531708,0.0106995851133921,
1.20835951516466));
#15171=CARTESIAN_POINT('Ctrl Pts',(-0.146373054956946,0.000132657382717961,
1.20893449541571));
#15172=CARTESIAN_POINT('Origin',(0.,0.,0.));
#15173=CARTESIAN_POINT('',(-0.146120596765396,-4.14129048147555E-5,1.26606550458429));
#15174=CARTESIAN_POINT('',(-0.146109918970638,-1.0198006988139E-5,1.25893449541571));
#15175=CARTESIAN_POINT('',(-0.14635,-1.79227059055215E-17,0.));
#15176=CARTESIAN_POINT('Ctrl Pts',(-0.146120596765396,-4.14129048147555E-5,
1.26606550458429));
#15177=CARTESIAN_POINT('Ctrl Pts',(-0.14605219935785,0.0269443530192317,
1.26460351894424));
#15178=CARTESIAN_POINT('Ctrl Pts',(-0.138898723445843,0.053963836666407,
1.26314153330418));
#15179=CARTESIAN_POINT('Ctrl Pts',(-0.124882896249422,0.0767650581554474,
1.26167954766413));
#15180=CARTESIAN_POINT('Ctrl Pts',(-0.0995129464537159,0.118037388097231,
1.25903321778503));
#15181=CARTESIAN_POINT('Ctrl Pts',(-0.051658938874944,0.145488850208621,
1.25638688790592));
#15182=CARTESIAN_POINT('Ctrl Pts',(-0.00322440565727106,0.146554478394238,
1.25374055802682));
#15183=CARTESIAN_POINT('Ctrl Pts',(0.0452101275604033,0.147620106579856,
1.25109422814772));
#15184=CARTESIAN_POINT('Ctrl Pts',(0.0942251864169787,0.122299900839699,
1.24844789826862));
#15185=CARTESIAN_POINT('Ctrl Pts',(0.121385807331354,0.0821833176976391,
1.24580156838952));
#15186=CARTESIAN_POINT('Ctrl Pts',(0.148546428245729,0.0420667345555804,
1.24315523851041));
#15187=CARTESIAN_POINT('Ctrl Pts',(0.153852611217905,-0.0128462259883804,
1.24050890863131));
#15188=CARTESIAN_POINT('Ctrl Pts',(0.134875632820701,-0.0574210379606392,
1.23786257875221));
#15189=CARTESIAN_POINT('Ctrl Pts',(0.115898654423498,-0.101995849932898,
1.23521624887311));
#15190=CARTESIAN_POINT('Ctrl Pts',(0.0726385146569148,-0.136232513333455,
1.23256991899401));
#15191=CARTESIAN_POINT('Ctrl Pts',(0.0248960600935515,-0.144460368686643,
1.2299235891149));
#15192=CARTESIAN_POINT('Ctrl Pts',(-0.0228463944698117,-0.152688224039831,
1.2272772592358));
#15193=CARTESIAN_POINT('Ctrl Pts',(-0.0750711638299551,-0.134907271345651,
1.2246309293567));
#15194=CARTESIAN_POINT('Ctrl Pts',(-0.107874149410843,-0.0992561323957017,
1.2219845994776));
#15195=CARTESIAN_POINT('Ctrl Pts',(-0.132331163880887,-0.072675612185966,
1.2200115678465));
#15196=CARTESIAN_POINT('Ctrl Pts',(-0.145992019903337,-0.0361614337449312,
1.21803853621539));
#15197=CARTESIAN_POINT('Ctrl Pts',(-0.146318311025392,0.000133437649768732,
1.21606550458429));
#15198=CARTESIAN_POINT('Ctrl Pts',(-0.146373054956946,0.000132657382717961,
1.20893449541571));
#15199=CARTESIAN_POINT('Ctrl Pts',(-0.146020767276673,-0.0379538636644633,
1.21100690453892));
#15200=CARTESIAN_POINT('Ctrl Pts',(-0.130797424420382,-0.0762899498869128,
1.21307931366213));
#15201=CARTESIAN_POINT('Ctrl Pts',(-0.104081054125652,-0.103227285106232,
1.21515172278534));
#15202=CARTESIAN_POINT('Ctrl Pts',(-0.0699523514264828,-0.137638258418326,
1.2177991121596));
#15203=CARTESIAN_POINT('Ctrl Pts',(-0.0170685611947798,-0.153447990763203,
1.22044650153386));
#15204=CARTESIAN_POINT('Ctrl Pts',(0.0303468241642401,-0.143414812629152,
1.22309389090812));
#15205=CARTESIAN_POINT('Ctrl Pts',(0.0777622095232573,-0.133381634495101,
1.22574128028238));
#15206=CARTESIAN_POINT('Ctrl Pts',(0.119709190009594,-0.0975055458821257,
1.22838866965664));
#15207=CARTESIAN_POINT('Ctrl Pts',(0.136973893871985,-0.052219638220276,
1.2310360590309));
#15208=CARTESIAN_POINT('Ctrl Pts',(0.154238597734379,-0.00693373055842239,
1.23368344840516));
#15209=CARTESIAN_POINT('Ctrl Pts',(0.146821024972825,0.0477619961523044,
1.23633083777942));
#15210=CARTESIAN_POINT('Ctrl Pts',(0.118118804930222,0.0868140895256425,
1.23897822715368));
#15211=CARTESIAN_POINT('Ctrl Pts',(0.0894165848876198,0.125866182898978,
1.24162561652794));
#15212=CARTESIAN_POINT('Ctrl Pts',(0.0394297175639698,0.149274642934924,
1.2442730059022));
#15213=CARTESIAN_POINT('Ctrl Pts',(-0.00894524413350711,0.146317192515786,
1.24692039527646));
#15214=CARTESIAN_POINT('Ctrl Pts',(-0.0573202058309854,0.143359742096648,
1.24956778465072));
#15215=CARTESIAN_POINT('Ctrl Pts',(-0.104083261902292,0.114036381222425,
1.25221517402498));
#15216=CARTESIAN_POINT('Ctrl Pts',(-0.127814530591109,0.0717787154251623,
1.25486256339924));
#15217=CARTESIAN_POINT('Ctrl Pts',(-0.139981499518435,0.0501133037087236,
1.2562198740714));
#15218=CARTESIAN_POINT('Ctrl Pts',(-0.146094355379323,0.0250479932723348,
1.25757718474355));
#15219=CARTESIAN_POINT('Ctrl Pts',(-0.146109918970638,-1.0198006988139E-5,
1.25893449541571));
#15220=CARTESIAN_POINT('Origin',(0.,0.,0.));
#15221=CARTESIAN_POINT('',(-0.146470135615938,-0.000111966546850736,1.31606550458429));
#15222=CARTESIAN_POINT('',(-0.146410535958061,-0.000127756381200432,1.30893449541571));
#15223=CARTESIAN_POINT('',(-0.14635,-1.79227059055215E-17,0.));
#15224=CARTESIAN_POINT('Ctrl Pts',(-0.146470135615938,-0.000111966546850736,
1.31606550458429));
#15225=CARTESIAN_POINT('Ctrl Pts',(-0.146120207411574,0.0411799307449602,
1.31381483155218));
#15226=CARTESIAN_POINT('Ctrl Pts',(-0.127827491572984,0.0827431563937987,
1.31156415852007));
#15227=CARTESIAN_POINT('Ctrl Pts',(-0.0969137672218927,0.10998333351997,
1.30931348548796));
#15228=CARTESIAN_POINT('Ctrl Pts',(-0.0605655677022408,0.142012194937238,
1.30666715560886));
#15229=CARTESIAN_POINT('Ctrl Pts',(-0.00676890401288169,0.154239532672684,
1.30402082572976));
#15230=CARTESIAN_POINT('Ctrl Pts',(0.0398526445220406,0.14106870189023,
1.30137449585066));
#15231=CARTESIAN_POINT('Ctrl Pts',(0.0864741930569617,0.127897871107775,
1.29872816597155));
#15232=CARTESIAN_POINT('Ctrl Pts',(0.125920626437448,0.0893288718074177,
1.29608183609245));
#15233=CARTESIAN_POINT('Ctrl Pts',(0.14013669149516,0.0430153417578024,
1.29343550621335));
#15234=CARTESIAN_POINT('Ctrl Pts',(0.154352756552873,-0.00329818829181684,
1.29078917633425));
#15235=CARTESIAN_POINT('Ctrl Pts',(0.143338453287813,-0.0573562490906975,
1.28814284645515));
#15236=CARTESIAN_POINT('Ctrl Pts',(0.112135201594409,-0.0944156157243562,
1.28549651657604));
#15237=CARTESIAN_POINT('Ctrl Pts',(0.0809319499010078,-0.131474982358013,
1.28285018669694));
#15238=CARTESIAN_POINT('Ctrl Pts',(0.0295397497792676,-0.151535654826449,
1.28020385681784));
#15239=CARTESIAN_POINT('Ctrl Pts',(-0.0185183802362589,-0.1454155477333,
1.27755752693874));
#15240=CARTESIAN_POINT('Ctrl Pts',(-0.066576510251784,-0.139295440640151,
1.27491119705964));
#15241=CARTESIAN_POINT('Ctrl Pts',(-0.111300570161094,-0.106994553985419,
1.27226486718053));
#15242=CARTESIAN_POINT('Ctrl Pts',(-0.13221965410943,-0.0632975117719662,
1.26961853730143));
#15243=CARTESIAN_POINT('Ctrl Pts',(-0.141581826511298,-0.0437412423069929,
1.26843419306239));
#15244=CARTESIAN_POINT('Ctrl Pts',(-0.146176005022067,-0.0219023912433209,
1.26724984882334));
#15245=CARTESIAN_POINT('Ctrl Pts',(-0.146120596765396,-4.14129048147555E-5,
1.26606550458429));
#15246=CARTESIAN_POINT('Ctrl Pts',(-0.146109918970638,-1.0198006988139E-5,
1.25893449541571));
#15247=CARTESIAN_POINT('Ctrl Pts',(-0.146124711647138,-0.0238271763493914,
1.26022457411781));
#15248=CARTESIAN_POINT('Ctrl Pts',(-0.140631289159497,-0.0476377233371588,
1.26151465281992));
#15249=CARTESIAN_POINT('Ctrl Pts',(-0.129592576141605,-0.0685164391025303,
1.26280473152202));
#15250=CARTESIAN_POINT('Ctrl Pts',(-0.106939871696956,-0.111361957112663,
1.26545212089628));
#15251=CARTESIAN_POINT('Ctrl Pts',(-0.0609349815013302,-0.141861022412626,
1.26809951027054));
#15252=CARTESIAN_POINT('Ctrl Pts',(-0.0126505083952331,-0.146043496451057,
1.2707468996448));
#15253=CARTESIAN_POINT('Ctrl Pts',(0.0356339647108625,-0.150225970489488,
1.27339428901906));
#15254=CARTESIAN_POINT('Ctrl Pts',(0.0861980207274291,-0.128091853266388,
1.27604167839332));
#15255=CARTESIAN_POINT('Ctrl Pts',(0.11588072467734,-0.0897797074320025,
1.27868906776758));
#15256=CARTESIAN_POINT('Ctrl Pts',(0.145563428627253,-0.0514675615976161,
1.28133645714184));
#15257=CARTESIAN_POINT('Ctrl Pts',(0.154364780510509,0.00302261284805656,
1.2839838465161));
#15258=CARTESIAN_POINT('Ctrl Pts',(0.138253309066183,0.0487315170146188,
1.28663123589036));
#15259=CARTESIAN_POINT('Ctrl Pts',(0.122141837621857,0.0944404211811797,
1.28927862526462));
#15260=CARTESIAN_POINT('Ctrl Pts',(0.0811175428499519,0.131368055068631,
1.29192601463888));
#15261=CARTESIAN_POINT('Ctrl Pts',(0.0339716590485425,0.142599665496764,
1.29457340401314));
#15262=CARTESIAN_POINT('Ctrl Pts',(-0.013174224752867,0.153831275924897,
1.2972207933874));
#15263=CARTESIAN_POINT('Ctrl Pts',(-0.0664416975837803,0.139366862893713,
1.29986818276166));
#15264=CARTESIAN_POINT('Ctrl Pts',(-0.101431520699135,0.105831870563862,
1.30251557213592));
#15265=CARTESIAN_POINT('Ctrl Pts',(-0.129710573305276,0.0787286237393239,
1.30465521322918));
#15266=CARTESIAN_POINT('Ctrl Pts',(-0.146050663974784,0.0391684733249047,
1.30679485432245));
#15267=CARTESIAN_POINT('Ctrl Pts',(-0.146410535958061,-0.000127756381200432,
1.30893449541571));
#15268=CARTESIAN_POINT('Origin',(0.,0.,0.));
#15269=CARTESIAN_POINT('',(-0.146471469669193,0.000111495080380188,1.36606550458429));
#15270=CARTESIAN_POINT('',(-0.146526884620975,8.5711493927648E-5,1.35893449541571));
#15271=CARTESIAN_POINT('',(-0.14635,-1.79227059055215E-17,0.));
#15272=CARTESIAN_POINT('Ctrl Pts',(-0.146471469669193,0.000111495080380188,
1.36606550458429));
#15273=CARTESIAN_POINT('Ctrl Pts',(-0.146532402405025,0.0073220458586883,
1.36567247403923));
#15274=CARTESIAN_POINT('Ctrl Pts',(-0.146045973070864,0.0145243451116175,
1.36527944349416));
#15275=CARTESIAN_POINT('Ctrl Pts',(-0.144983764805735,0.0216407019395156,
1.3648864129491));
#15276=CARTESIAN_POINT('Ctrl Pts',(-0.137831767320671,0.0695561322809842,
1.36224008307));
#15277=CARTESIAN_POINT('Ctrl Pts',(-0.104576727819841,0.113575347233418,
1.3595937531909));
#15278=CARTESIAN_POINT('Ctrl Pts',(-0.060440002550743,0.133550058215342,
1.3569474233118));
#15279=CARTESIAN_POINT('Ctrl Pts',(-0.0163032772816473,0.153524769197265,
1.35430109343269));
#15280=CARTESIAN_POINT('Ctrl Pts',(0.0387151337557165,0.149454976208681,
1.35165476355359));
#15281=CARTESIAN_POINT('Ctrl Pts',(0.0794324390145508,0.123203488242689,
1.34900843367449));
#15282=CARTESIAN_POINT('Ctrl Pts',(0.120149744273387,0.0969520002766962,
1.34636210379539));
#15283=CARTESIAN_POINT('Ctrl Pts',(0.146565943753694,0.048518817333291,
1.34371577391629));
#15284=CARTESIAN_POINT('Ctrl Pts',(0.14658992694451,7.25688577880009E-5,
1.34106944403718));
#15285=CARTESIAN_POINT('Ctrl Pts',(0.146613910135327,-0.0483736796177136,
1.33842311415808));
#15286=CARTESIAN_POINT('Ctrl Pts',(0.120245677036657,-0.0968329936253116,
1.33577678427898));
#15287=CARTESIAN_POINT('Ctrl Pts',(0.0795543829983497,-0.123124782547022,
1.33313045439988));
#15288=CARTESIAN_POINT('Ctrl Pts',(0.0388630889600415,-0.149416571468734,
1.33048412452078));
#15289=CARTESIAN_POINT('Ctrl Pts',(-0.0161512660179049,-0.153540835304554,
1.32783779464168));
#15290=CARTESIAN_POINT('Ctrl Pts',(-0.0603077462478081,-0.133609833714981,
1.32519146476257));
#15291=CARTESIAN_POINT('Ctrl Pts',(-0.10446422647771,-0.113678832125408,
1.32254513488347));
#15292=CARTESIAN_POINT('Ctrl Pts',(-0.137762831959571,-0.0696925651104417,
1.31989880500437));
#15293=CARTESIAN_POINT('Ctrl Pts',(-0.144962267025529,-0.0217842390534145,
1.31725247512527));
#15294=CARTESIAN_POINT('Ctrl Pts',(-0.146038665626028,-0.0146213916011371,
1.31685681827827));
#15295=CARTESIAN_POINT('Ctrl Pts',(-0.146531651210624,-0.00737087161912708,
1.31646116143128));
#15296=CARTESIAN_POINT('Ctrl Pts',(-0.146470135615938,-0.000111966546850736,
1.31606550458429));
#15297=CARTESIAN_POINT('Ctrl Pts',(-0.146410535958061,-0.000127756381200432,
1.30893449541571));
#15298=CARTESIAN_POINT('Ctrl Pts',(-0.146495935505426,-0.00945296197092968,
1.30944224369671));
#15299=CARTESIAN_POINT('Ctrl Pts',(-0.145681427739287,-0.018763305174839,
1.3099499919777));
#15300=CARTESIAN_POINT('Ctrl Pts',(-0.143913007029536,-0.0278887903271487,
1.3104577402587));
#15301=CARTESIAN_POINT('Ctrl Pts',(-0.134692496844786,-0.0754688872597875,
1.31310512963296));
#15302=CARTESIAN_POINT('Ctrl Pts',(-0.0995393030754929,-0.118023509496548,
1.31575251900722));
#15303=CARTESIAN_POINT('Ctrl Pts',(-0.0545553941775042,-0.136060454153345,
1.31839990838148));
#15304=CARTESIAN_POINT('Ctrl Pts',(-0.00957148527951295,-0.154097398810142,
1.32104729775574));
#15305=CARTESIAN_POINT('Ctrl Pts',(0.0452431387471776,-0.14761666588697,
1.32369468713));
#15306=CARTESIAN_POINT('Ctrl Pts',(0.0847805644327026,-0.119586763955155,
1.32634207650426));
#15307=CARTESIAN_POINT('Ctrl Pts',(0.124317990118227,-0.09155686202334,
1.32898946587852));
#15308=CARTESIAN_POINT('Ctrl Pts',(0.148578217462589,-0.041977791082884,
1.33163685525278));
#15309=CARTESIAN_POINT('Ctrl Pts',(0.146448816178573,0.00644068764408242,
1.33428424462704));
#15310=CARTESIAN_POINT('Ctrl Pts',(0.144319414894557,0.0548591663710502,
1.3369316340013));
#15311=CARTESIAN_POINT('Ctrl Pts',(0.115800384982161,0.102117052884526,
1.33957902337556));
#15312=CARTESIAN_POINT('Ctrl Pts',(0.0739549070570988,0.126567807678519,
1.34222641274982));
#15313=CARTESIAN_POINT('Ctrl Pts',(0.0321094291320376,0.151018562472512,
1.34487380212408));
#15314=CARTESIAN_POINT('Ctrl Pts',(-0.0230624968056921,0.152662185547021,
1.34752119149834));
#15315=CARTESIAN_POINT('Ctrl Pts',(-0.0662892946253695,0.1307458130856,
1.3501685808726));
#15316=CARTESIAN_POINT('Ctrl Pts',(-0.109516092445046,0.10882944062418,
1.35281597024686));
#15317=CARTESIAN_POINT('Ctrl Pts',(-0.140797762146673,0.0633530726268328,
1.35546335962112));
#15318=CARTESIAN_POINT('Ctrl Pts',(-0.145805692234247,0.0151472216574969,
1.35811074899538));
#15319=CARTESIAN_POINT('Ctrl Pts',(-0.146325105122407,0.0101474034011793,
1.35838533113549));
#15320=CARTESIAN_POINT('Ctrl Pts',(-0.146561879835735,0.00511822289583405,
1.3586599132756));
#15321=CARTESIAN_POINT('Ctrl Pts',(-0.146526884620975,8.5711493927648E-5,
1.35893449541571));
#15322=CARTESIAN_POINT('Origin',(0.,0.,0.));
#15323=CARTESIAN_POINT('',(-0.146120987371435,4.2191387702159E-5,1.41606550458429));
#15324=CARTESIAN_POINT('',(-0.146148882937928,7.6306569664006E-5,1.40893449541571));
#15325=CARTESIAN_POINT('',(-0.14635,-1.79227059055215E-17,0.));
#15326=CARTESIAN_POINT('Ctrl Pts',(-0.146120987371435,4.2191387702159E-5,
1.41606550458429));
#15327=CARTESIAN_POINT('Ctrl Pts',(-0.146177309023295,0.021854523983563,
1.41488378664717));
#15328=CARTESIAN_POINT('Ctrl Pts',(-0.141604359564088,0.0436444172696427,
1.41370206871005));
#15329=CARTESIAN_POINT('Ctrl Pts',(-0.132282279973341,0.0631665524487371,
1.41252035077294));
#15330=CARTESIAN_POINT('Ctrl Pts',(-0.1114064880593,0.106884268839086,1.40987402089383));
#15331=CARTESIAN_POINT('Ctrl Pts',(-0.0667143915920224,0.139229456738304,
1.40722769101473));
#15332=CARTESIAN_POINT('Ctrl Pts',(-0.0186623352932378,0.145397151366753,
1.40458136113563));
#15333=CARTESIAN_POINT('Ctrl Pts',(0.0293897210055454,0.151564845995202,
1.40193503125653));
#15334=CARTESIAN_POINT('Ctrl Pts',(0.0808017371358351,0.131555047352884,
1.39928870137743));
#15335=CARTESIAN_POINT('Ctrl Pts',(0.112041660826149,0.0945265884816804,
1.39664237149832));
#15336=CARTESIAN_POINT('Ctrl Pts',(0.143281584516463,0.0574981296104763,
1.39399604161922));
#15337=CARTESIAN_POINT('Ctrl Pts',(0.154349415766802,0.00345101051038574,
1.39134971174012));
#15338=CARTESIAN_POINT('Ctrl Pts',(0.140179214932283,-0.0428765696854336,
1.38870338186102));
#15339=CARTESIAN_POINT('Ctrl Pts',(0.126009014097764,-0.089204149881253,
1.38605705198192));
#15340=CARTESIAN_POINT('Ctrl Pts',(0.0866007811783877,-0.127812191172801,
1.38341072210282));
#15341=CARTESIAN_POINT('Ctrl Pts',(0.0399922944706322,-0.14102917638501,
1.38076439222371));
#15342=CARTESIAN_POINT('Ctrl Pts',(-0.00661619223712474,-0.15424616159722,
1.37811806234461));
#15343=CARTESIAN_POINT('Ctrl Pts',(-0.060424932733261,-0.142072090730089,
1.37547173246551));
#15344=CARTESIAN_POINT('Ctrl Pts',(-0.0968048252466797,-0.110079232431271,
1.37282540258641));
#15345=CARTESIAN_POINT('Ctrl Pts',(-0.127781608685608,-0.08283792481198,
1.37057210325237));
#15346=CARTESIAN_POINT('Ctrl Pts',(-0.146122133733866,-0.0412276055847571,
1.36831880391833));
#15347=CARTESIAN_POINT('Ctrl Pts',(-0.146471469669193,0.000111495080380188,
1.36606550458429));
#15348=CARTESIAN_POINT('Ctrl Pts',(-0.146526884620975,8.5711493927648E-5,
1.35893449541571));
#15349=CARTESIAN_POINT('Ctrl Pts',(-0.146224472749943,-0.0434028397118431,
1.36130730264986));
#15350=CARTESIAN_POINT('Ctrl Pts',(-0.125627402569456,-0.0871401285467012,
1.36368010988401));
#15351=CARTESIAN_POINT('Ctrl Pts',(-0.0917490966422633,-0.114327780902106,
1.36605291711816));
#15352=CARTESIAN_POINT('Ctrl Pts',(-0.0539503804891888,-0.144661598551044,
1.36870030649242));
#15353=CARTESIAN_POINT('Ctrl Pts',(0.00038124229047478,-0.154393899907594,
1.37134769586668));
#15354=CARTESIAN_POINT('Ctrl Pts',(0.0463590973565905,-0.139066790892088,
1.37399508524094));
#15355=CARTESIAN_POINT('Ctrl Pts',(0.0923369524227062,-0.123739681876581,
1.3766424746152));
#15356=CARTESIAN_POINT('Ctrl Pts',(0.129961039775272,-0.083353162489017,
1.37928986398946));
#15357=CARTESIAN_POINT('Ctrl Pts',(0.141997595260484,-0.0364063334065561,
1.38193725336372));
#15358=CARTESIAN_POINT('Ctrl Pts',(0.154034150745695,0.0105404956759021,
1.38458464273798));
#15359=CARTESIAN_POINT('Ctrl Pts',(0.140483174363557,0.0640476344532581,
1.38723203211224));
#15360=CARTESIAN_POINT('Ctrl Pts',(0.10755170844225,0.0996060653705087,
1.3898794214865));
#15361=CARTESIAN_POINT('Ctrl Pts',(0.0746202425209409,0.135164496287762,
1.39252681086076));
#15362=CARTESIAN_POINT('Ctrl Pts',(0.0223082870604623,0.152774219344908,
1.39517420023502));
#15363=CARTESIAN_POINT('Ctrl Pts',(-0.025422593472234,0.144369075867769,
1.39782158960928));
#15364=CARTESIAN_POINT('Ctrl Pts',(-0.073153474004929,0.135963932390631,
1.40046897898354));
#15365=CARTESIAN_POINT('Ctrl Pts',(-0.11630327960984,0.101543922379208,
1.4031163683578));
#15366=CARTESIAN_POINT('Ctrl Pts',(-0.135107186188192,0.0568751802851974,
1.40576375773206));
#15367=CARTESIAN_POINT('Ctrl Pts',(-0.142614236437708,0.0390421576584788,
1.40682067029328));
#15368=CARTESIAN_POINT('Ctrl Pts',(-0.14624095998336,0.0195756595648056,
1.40787758285449));
#15369=CARTESIAN_POINT('Ctrl Pts',(-0.146148882937928,7.6306569664006E-5,
1.40893449541571));
#15370=CARTESIAN_POINT('Origin',(0.,0.,0.));
#15371=CARTESIAN_POINT('',(-0.14631473222987,-0.000131398079681141,1.46606550458429));
#15372=CARTESIAN_POINT('',(-0.146248097568756,-0.000123763188177425,1.45893449541571));
#15373=CARTESIAN_POINT('',(-0.14635,-1.79227059055215E-17,0.));
#15374=CARTESIAN_POINT('Ctrl Pts',(-0.14631473222987,-0.000131398079681141,
1.46606550458429));
#15375=CARTESIAN_POINT('Ctrl Pts',(-0.145989697979493,0.0361157155227289,
1.46409509925512));
#15376=CARTESIAN_POINT('Ctrl Pts',(-0.132370868650209,0.0725796635271419,
1.46212469392594));
#15377=CARTESIAN_POINT('Ctrl Pts',(-0.107973319296019,0.0991484059484618,
1.46015428859677));
#15378=CARTESIAN_POINT('Ctrl Pts',(-0.0752064754000165,0.134831245351468,
1.45750795871767));
#15379=CARTESIAN_POINT('Ctrl Pts',(-0.0229974942306327,0.152665588379184,
1.45486162883857));
#15380=CARTESIAN_POINT('Ctrl Pts',(0.0247535192036911,0.144485406820094,
1.45221529895946));
#15381=CARTESIAN_POINT('Ctrl Pts',(0.0725045326380122,0.136305225261004,
1.44956896908036));
#15382=CARTESIAN_POINT('Ctrl Pts',(0.115797578337275,0.102110519115111,
1.44692263920126));
#15383=CARTESIAN_POINT('Ctrl Pts',(0.134818450998255,0.0575543070937695,
1.44427630932216));
#15384=CARTESIAN_POINT('Ctrl Pts',(0.153839323659235,0.0129980950724284,
1.44162997944306));
#15385=CARTESIAN_POINT('Ctrl Pts',(0.148588023281934,-0.0419196228243577,
1.43898364956396));
#15386=CARTESIAN_POINT('Ctrl Pts',(0.121467255745355,-0.082062966762292,
1.43633731968485));
#15387=CARTESIAN_POINT('Ctrl Pts',(0.0943464882087764,-0.122206310700226,
1.43369098980575));
#15388=CARTESIAN_POINT('Ctrl Pts',(0.0453562535129183,-0.147575280679306,
1.43104465992665));
#15389=CARTESIAN_POINT('Ctrl Pts',(-0.00307937473935208,-0.146557666176543,
1.42839833004755));
#15390=CARTESIAN_POINT('Ctrl Pts',(-0.0515150029916225,-0.14554005167378,
1.42575200016845));
#15391=CARTESIAN_POINT('Ctrl Pts',(-0.0993960248003067,-0.118135852689175,
1.42310567028934));
#15392=CARTESIAN_POINT('Ctrl Pts',(-0.124806792024246,-0.0768886307561326,
1.42045934041024));
#15393=CARTESIAN_POINT('Ctrl Pts',(-0.138870387581649,-0.0540603453281256,
1.41899472846826));
#15394=CARTESIAN_POINT('Ctrl Pts',(-0.146051182757901,-0.0269918425378075,
1.41753011652627));
#15395=CARTESIAN_POINT('Ctrl Pts',(-0.146120987371435,4.2191387702159E-5,
1.41606550458429));
#15396=CARTESIAN_POINT('Ctrl Pts',(-0.146148882937928,7.6306569664006E-5,
1.40893449541571));
#15397=CARTESIAN_POINT('Ctrl Pts',(-0.146010322369016,-0.0292669616874671,
1.41052497222875));
#15398=CARTESIAN_POINT('Ctrl Pts',(-0.137450455640384,-0.0586846305953837,
1.4121154490418));
#15399=CARTESIAN_POINT('Ctrl Pts',(-0.121019719714466,-0.0827222215753489,
1.41370592585484));
#15400=CARTESIAN_POINT('Ctrl Pts',(-0.0936703391105966,-0.122733407165291,
1.4163533152291));
#15401=CARTESIAN_POINT('Ctrl Pts',(-0.0445135703510636,-0.147838304168576,
1.41900070460336));
#15402=CARTESIAN_POINT('Ctrl Pts',(0.00393424939099551,-0.146537573651384,
1.42164809397762));
#15403=CARTESIAN_POINT('Ctrl Pts',(0.0523820691330518,-0.145236843134192,
1.42429548335188));
#15404=CARTESIAN_POINT('Ctrl Pts',(0.100120939857634,-0.117530485096527,
1.42694287272614));
#15405=CARTESIAN_POINT('Ctrl Pts',(0.125284029446909,-0.0761094471358441,
1.4295902621004));
#15406=CARTESIAN_POINT('Ctrl Pts',(0.150447119036187,-0.0346884091751576,
1.43223765147466));
#15407=CARTESIAN_POINT('Ctrl Pts',(0.153034427490153,0.020447308708549,
1.43488504084892));
#15408=CARTESIAN_POINT('Ctrl Pts',(0.13186079120536,0.0640427391611241,
1.43753243022318));
#15409=CARTESIAN_POINT('Ctrl Pts',(0.110687154920568,0.107638169613697,
1.44017981959744));
#15410=CARTESIAN_POINT('Ctrl Pts',(0.0657525738970213,0.139693312635139,
1.4428272089717));
#15411=CARTESIAN_POINT('Ctrl Pts',(0.0176394768514684,0.145525221357757,
1.44547459834596));
#15412=CARTESIAN_POINT('Ctrl Pts',(-0.0304736201940859,0.151357130080375,
1.44812198772022));
#15413=CARTESIAN_POINT('Ctrl Pts',(-0.0817652332616461,0.130965804504167,
1.45076937709448));
#15414=CARTESIAN_POINT('Ctrl Pts',(-0.112741325423428,0.0936916042199666,
1.45341676646874));
#15415=CARTESIAN_POINT('Ctrl Pts',(-0.134261605244105,0.0677957870194472,
1.45525600945106));
#15416=CARTESIAN_POINT('Ctrl Pts',(-0.145976367207401,0.0337512577971725,
1.45709525243339));
#15417=CARTESIAN_POINT('Ctrl Pts',(-0.146248097568756,-0.000123763188177425,
1.45893449541571));
#15418=CARTESIAN_POINT('Origin',(0.,0.,-0.0924367114736175));
#15419=CARTESIAN_POINT('',(-0.117746618301147,-0.000105742458702955,1.48256328852638));
#15420=CARTESIAN_POINT('',(-0.117971241274414,-5.28325160115065E-6,1.49243671147361));
#15421=CARTESIAN_POINT('',(-0.117775,2.85464118895969E-14,-0.0924367114736175));
#15422=CARTESIAN_POINT('',(-0.117668597464313,0.00500517689812599,1.532225));
#15423=CARTESIAN_POINT('Ctrl Pts',(-0.117746618301147,-0.000105742458702949,
1.48256328852638));
#15424=CARTESIAN_POINT('Ctrl Pts',(-0.117836347163251,-0.0101121102621826,
1.48323921307631));
#15425=CARTESIAN_POINT('Ctrl Pts',(-0.112089674709738,-0.0591937430214443,
1.48656146750534));
#15426=CARTESIAN_POINT('Ctrl Pts',(-0.0435804807853106,-0.132222740314769,
1.49253005181348));
#15427=CARTESIAN_POINT('Ctrl Pts',(0.0874774386997331,-0.108286040948335,
1.50046904145078));
#15428=CARTESIAN_POINT('Ctrl Pts',(0.138385550162814,0.0147146982980264,
1.50840803108809));
#15429=CARTESIAN_POINT('Ctrl Pts',(0.0627460642121078,0.124368470664037,
1.51634702072539));
#15430=CARTESIAN_POINT('Ctrl Pts',(-0.0706026869052757,0.119928391791904,
1.5242860103627));
#15431=CARTESIAN_POINT('Ctrl Pts',(-0.116004137797729,0.0441355889673283,
1.5295786701209));
#15432=CARTESIAN_POINT('Ctrl Pts',(-0.117668597464313,0.00500517689812487,
1.532225));
#15433=CARTESIAN_POINT('',(-0.0334019664627544,0.1129391839063,1.53222500000001));
#15434=CARTESIAN_POINT('Origin',(0.,0.,1.532225));
#15435=CARTESIAN_POINT('Ctrl Pts',(-0.117971276761593,-5.28420699491729E-6,
1.49243671147361));
#15436=CARTESIAN_POINT('Ctrl Pts',(-0.117971582784674,-0.000385634193345565,
1.49246252744444));
#15437=CARTESIAN_POINT('Ctrl Pts',(-0.117794795258817,-0.0397700451254522,
1.49513573278954));
#15438=CARTESIAN_POINT('Ctrl Pts',(-0.0742871760264013,-0.117748889605885,
1.50045632750888));
#15439=CARTESIAN_POINT('Ctrl Pts',(0.0586284551779338,-0.126233948370975,
1.50839849563167));
#15440=CARTESIAN_POINT('Ctrl Pts',(0.137995068118234,-0.019163470063063,
1.51634066375444));
#15441=CARTESIAN_POINT('Ctrl Pts',(0.0906261803825392,0.105639137646141,
1.52428283187723));
#15442=CARTESIAN_POINT('Ctrl Pts',(0.00417072711528833,0.124051375507138,
1.52957761062575));
#15443=CARTESIAN_POINT('Ctrl Pts',(-0.0334019664627544,0.1129391839063,
1.53222500000001));
#15444=CARTESIAN_POINT('Origin',(0.,0.,-0.0924367114736175));
#15445=CARTESIAN_POINT('',(-0.117590702341447,3.3953472435133E-5,1.43256328852638));
#15446=CARTESIAN_POINT('',(-0.117692994131604,-9.95982882293356E-5,1.44243671147361));
#15447=CARTESIAN_POINT('',(-0.117775,2.85464118895969E-14,-0.0924367114736175));
#15448=CARTESIAN_POINT('Ctrl Pts',(-0.117590702341447,3.39534724351446E-5,
1.43256328852638));
#15449=CARTESIAN_POINT('Ctrl Pts',(-0.117534527156218,-0.0217216553118358,
1.43402790046837));
#15450=CARTESIAN_POINT('Ctrl Pts',(-0.101314495966545,-0.0828641818343832,
1.43813884228945));
#15451=CARTESIAN_POINT('Ctrl Pts',(-0.00292444232197888,-0.139176693688359,
1.44489611398964));
#15452=CARTESIAN_POINT('Ctrl Pts',(0.115350068603298,-0.0779297424218237,
1.45283510362695));
#15453=CARTESIAN_POINT('Ctrl Pts',(0.128028003046829,0.0546551750765237,
1.46077409326425));
#15454=CARTESIAN_POINT('Ctrl Pts',(0.0235079116789307,0.137209630484779,
1.46871308290156));
#15455=CARTESIAN_POINT('Ctrl Pts',(-0.0918059616614023,0.0978189523496558,
1.47597614798894));
#15456=CARTESIAN_POINT('Ctrl Pts',(-0.117485047349053,0.0290640819657798,
1.48059288319721));
#15457=CARTESIAN_POINT('Ctrl Pts',(-0.117746618301147,-0.000105742458702949,
1.48256328852638));
#15458=CARTESIAN_POINT('Ctrl Pts',(-0.117692994131604,-9.9598288229346E-5,
1.44243671147361));
#15459=CARTESIAN_POINT('Ctrl Pts',(-0.117789077779518,-0.0120777797952868,
1.44324485786555));
#15460=CARTESIAN_POINT('Ctrl Pts',(-0.110597905189529,-0.0631824179582176,
1.44670039363175));
#15461=CARTESIAN_POINT('Ctrl Pts',(-0.0368790902657646,-0.134252921254984,
1.45280331877221));
#15462=CARTESIAN_POINT('Ctrl Pts',(0.0928396680879532,-0.103751556080299,
1.46074548689499));
#15463=CARTESIAN_POINT('Ctrl Pts',(0.137511141307062,0.0217950526079239,
1.46868765501776));
#15464=CARTESIAN_POINT('Ctrl Pts',(0.0562018483347667,0.127378648737854,
1.47662982314055));
#15465=CARTESIAN_POINT('Ctrl Pts',(-0.0761502833827582,0.1162998103107,
1.48454617529249));
#15466=CARTESIAN_POINT('Ctrl Pts',(-0.117940200573233,0.0386186906477724,
1.48981513807018));
#15467=CARTESIAN_POINT('Ctrl Pts',(-0.117971276761593,-5.28420699491729E-6,
1.49243671147361));
#15468=CARTESIAN_POINT('Origin',(0.,0.,-0.0924367114736175));
#15469=CARTESIAN_POINT('',(-0.117872752581409,8.97255421561373E-5,1.38256328852638));
#15470=CARTESIAN_POINT('',(-0.117613151267609,6.14076272390171E-5,1.39243671147361));
#15471=CARTESIAN_POINT('',(-0.117775,2.85464118895969E-14,-0.0924367114736175));
#15472=CARTESIAN_POINT('Ctrl Pts',(-0.117872752581409,8.97255421561322E-5,
1.38256328852638));
#15473=CARTESIAN_POINT('Ctrl Pts',(-0.117591624875346,-0.0331778698171688,
1.38481658786042));
#15474=CARTESIAN_POINT('Ctrl Pts',(-0.0854981695600773,-0.105990339321694,
1.38971621707357));
#15475=CARTESIAN_POINT('Ctrl Pts',(0.0379781508110965,-0.133926497290667,
1.39726217616581));
#15476=CARTESIAN_POINT('Ctrl Pts',(0.133119345865688,-0.0407171622080862,
1.40520116580311));
#15477=CARTESIAN_POINT('Ctrl Pts',(0.106398871137127,0.0897659150453452,
1.41314015544042));
#15478=CARTESIAN_POINT('Ctrl Pts',(-0.0177224175491345,0.138074504763813,
1.42107914507772));
#15479=CARTESIAN_POINT('Ctrl Pts',(-0.105714817800915,0.0743914165933911,
1.42755352277305));
#15480=CARTESIAN_POINT('Ctrl Pts',(-0.11763602712824,0.0175874039095825,
1.43138157058926));
#15481=CARTESIAN_POINT('Ctrl Pts',(-0.117590702341447,3.39534724351446E-5,
1.43256328852638));
#15482=CARTESIAN_POINT('Ctrl Pts',(-0.117613151267609,6.1407627239024E-5,
1.39243671147361));
#15483=CARTESIAN_POINT('Ctrl Pts',(-0.117501644803633,-0.0235525549213426,
1.39402718828666));
#15484=CARTESIAN_POINT('Ctrl Pts',(-0.0991469449676741,-0.0866320980727062,
1.39826505447396));
#15485=CARTESIAN_POINT('Ctrl Pts',(0.00373660876362508,-0.139175849115243,
1.40515031003553));
#15486=CARTESIAN_POINT('Ctrl Pts',(0.118990018389619,-0.0722858665142316,
1.41309247815831));
#15487=CARTESIAN_POINT('Ctrl Pts',(0.125236419206141,0.0608253567263532,
1.42103464628109));
#15488=CARTESIAN_POINT('Ctrl Pts',(0.0167532566496359,0.13821437898841,
1.42897681440387));
#15489=CARTESIAN_POINT('Ctrl Pts',(-0.0944771051913143,0.0939940009069027,
1.43611083613471));
#15490=CARTESIAN_POINT('Ctrl Pts',(-0.117474319425011,0.0271612872365273,
1.44059746849129));
#15491=CARTESIAN_POINT('Ctrl Pts',(-0.117692994131604,-9.9598288229346E-5,
1.44243671147361));
#15492=CARTESIAN_POINT('Origin',(0.,0.,-0.0924367114736175));
#15493=CARTESIAN_POINT('',(-0.117871679003533,-9.01049542302267E-5,1.33256328852638));
#15494=CARTESIAN_POINT('',(-0.117917347702326,6.89762296073142E-5,1.34243671147361));
#15495=CARTESIAN_POINT('',(-0.117775,2.85464118895969E-14,-0.0924367114736175));
#15496=CARTESIAN_POINT('Ctrl Pts',(-0.117871679003533,-9.01049542302501E-5,
1.33256328852638));
#15497=CARTESIAN_POINT('Ctrl Pts',(-0.117921183610054,-0.00593170075121234,
1.33295894537338));
#15498=CARTESIAN_POINT('Ctrl Pts',(-0.114870949065289,-0.0507926200311143,
1.33600093209947));
#15499=CARTESIAN_POINT('Ctrl Pts',(-0.0572704544775333,-0.126880813469472,
1.34168924870467));
#15500=CARTESIAN_POINT('Ctrl Pts',(0.0755477687720905,-0.116923823242002,
1.34962823834197));
#15501=CARTESIAN_POINT('Ctrl Pts',(0.13920718769651,6.89141801743488E-5,
1.35756722797928));
#15502=CARTESIAN_POINT('Ctrl Pts',(0.0754319660950179,0.116998564767658,
1.36550621761658));
#15503=CARTESIAN_POINT('Ctrl Pts',(-0.0573960494825499,0.126824048933643,
1.37344520725389));
#15504=CARTESIAN_POINT('Ctrl Pts',(-0.11489462347839,0.0507140179075799,
1.37913089755716));
#15505=CARTESIAN_POINT('Ctrl Pts',(-0.117921788132912,0.00589240827474643,
1.38217025798132));
#15506=CARTESIAN_POINT('Ctrl Pts',(-0.117872752581409,8.97255421561322E-5,
1.38256328852638));
#15507=CARTESIAN_POINT('Ctrl Pts',(-0.117917347702326,6.89762296073276E-5,
1.34243671147361));
#15508=CARTESIAN_POINT('Ctrl Pts',(-0.117673982084908,-0.0349283870656527,
1.34480951870776));
#15509=CARTESIAN_POINT('Ctrl Pts',(-0.0826049238592893,-0.109396528181867,
1.34982971531618));
#15510=CARTESIAN_POINT('Ctrl Pts',(0.0440301174146577,-0.132080378229483,
1.35749730129884));
#15511=CARTESIAN_POINT('Ctrl Pts',(0.13486394497766,-0.0345773583278084,
1.36543946942163));
#15512=CARTESIAN_POINT('Ctrl Pts',(0.102148545386143,0.0946020732301706,
1.3733816375444));
#15513=CARTESIAN_POINT('Ctrl Pts',(-0.0241454188302812,0.137116288461919,
1.38132380566719));
#15514=CARTESIAN_POINT('Ctrl Pts',(-0.107458038693719,0.07065895059964,
1.38767549697692));
#15515=CARTESIAN_POINT('Ctrl Pts',(-0.117687250167678,0.015753490298928,
1.3913797989124));
#15516=CARTESIAN_POINT('Ctrl Pts',(-0.117613151267609,6.1407627239024E-5,
1.39243671147361));
#15517=CARTESIAN_POINT('Origin',(0.,0.,-0.0924367114736175));
#15518=CARTESIAN_POINT('',(-0.117590388001671,-3.33269891443968E-5,1.28256328852638));
#15519=CARTESIAN_POINT('',(-0.117823716245033,-0.000102811805890834,1.29243671147362));
#15520=CARTESIAN_POINT('',(-0.117775,2.85464118895969E-14,-0.0924367114736175));
#15521=CARTESIAN_POINT('Ctrl Pts',(-0.117590388001671,-3.33269891444124E-5,
1.28256328852638));
#15522=CARTESIAN_POINT('Ctrl Pts',(-0.117634977734708,-0.017625925033684,
1.28374763276543));
#15523=CARTESIAN_POINT('Ctrl Pts',(-0.105676786131388,-0.0744702911817869,
1.28757830688358));
#15524=CARTESIAN_POINT('Ctrl Pts',(-0.0175857351491984,-0.138091953858251,
1.29405531088083));
#15525=CARTESIAN_POINT('Ctrl Pts',(0.106487712804436,-0.089660542174548,
1.30199430051814));
#15526=CARTESIAN_POINT('Ctrl Pts',(0.133078957772855,0.0408489510387311,
1.30993329015544));
#15527=CARTESIAN_POINT('Ctrl Pts',(0.0378455373822902,0.133964029124136,
1.31787227979275));
#15528=CARTESIAN_POINT('Ctrl Pts',(-0.0855601048685178,0.105915403748908,
1.32541561258306));
#15529=CARTESIAN_POINT('Ctrl Pts',(-0.117590074669608,0.0331395035428114,
1.33031261549427));
#15530=CARTESIAN_POINT('Ctrl Pts',(-0.117871679003533,-9.01049542302501E-5,
1.33256328852638));
#15531=CARTESIAN_POINT('Ctrl Pts',(-0.117823716245033,-0.000102811805890825,
1.29243671147362));
#15532=CARTESIAN_POINT('Ctrl Pts',(-0.117892441435953,-0.00760726064997237,
1.29294445975461));
#15533=CARTESIAN_POINT('Ctrl Pts',(-0.113819337750002,-0.0541654333254181,
1.29609959740987));
#15534=CARTESIAN_POINT('Ctrl Pts',(-0.0518146499729274,-0.129225073214149,
1.30190212443939));
#15535=CARTESIAN_POINT('Ctrl Pts',(0.0805213734929343,-0.11357898534207,
1.30984429256217));
#15536=CARTESIAN_POINT('Ctrl Pts',(0.1390915465469,0.0061171215252809,1.31778646068495));
#15537=CARTESIAN_POINT('Ctrl Pts',(0.0702395735793815,0.120209316621791,
1.32572862880773));
#15538=CARTESIAN_POINT('Ctrl Pts',(-0.0629590648350173,0.124177428154433,
1.33367079693051));
#15539=CARTESIAN_POINT('Ctrl Pts',(-0.115917830154768,0.0471875384414626,
1.33924015781913));
#15540=CARTESIAN_POINT('Ctrl Pts',(-0.117945510062545,0.00411888419242175,
1.3421621293335));
#15541=CARTESIAN_POINT('Ctrl Pts',(-0.117917347702326,6.89762296073276E-5,
1.34243671147361));
#15542=CARTESIAN_POINT('Origin',(0.,0.,-0.0924367114736175));
#15543=CARTESIAN_POINT('',(-0.11774949833287,0.000107383800510985,1.23256328852638));
#15544=CARTESIAN_POINT('',(-0.117581795058195,-8.20683476789735E-6,1.24243671147361));
#15545=CARTESIAN_POINT('',(-0.117775,2.85464118895969E-14,-0.0924367114736175));
#15546=CARTESIAN_POINT('Ctrl Pts',(-0.11774949833287,0.000107383800510997,
1.23256328852638));
#15547=CARTESIAN_POINT('Ctrl Pts',(-0.1174869159147,-0.0291008736543001,
1.23453632015749));
#15548=CARTESIAN_POINT('Ctrl Pts',(-0.0917482398636095,-0.0978979247776974,
1.23915568166769));
#15549=CARTESIAN_POINT('Ctrl Pts',(0.0236422145726536,-0.137184880695923,
1.246421373057));
#15550=CARTESIAN_POINT('Ctrl Pts',(0.128082862902196,-0.0545291301253663,
1.2543603626943));
#15551=CARTESIAN_POINT('Ctrl Pts',(0.115272428336817,0.0780443019497631,
1.26229935233161));
#15552=CARTESIAN_POINT('Ctrl Pts',(-0.00306201423577413,0.139173524314926,
1.27023834196891));
#15553=CARTESIAN_POINT('Ctrl Pts',(-0.101358337705897,0.08278581645186,
1.27699298736717));
#15554=CARTESIAN_POINT('Ctrl Pts',(-0.117535345263889,0.02168343817453,
1.28110130288633));
#15555=CARTESIAN_POINT('Ctrl Pts',(-0.117590388001671,-3.33269891444124E-5,
1.28256328852638));
#15556=CARTESIAN_POINT('Ctrl Pts',(-0.117581795058195,-8.20683476789562E-6,
1.24243671147361));
#15557=CARTESIAN_POINT('Ctrl Pts',(-0.117593699448189,-0.0191748937105988,
1.24372679017572));
#15558=CARTESIAN_POINT('Ctrl Pts',(-0.104100832827715,-0.0776580224685839,
1.24766425825208));
#15559=CARTESIAN_POINT('Ctrl Pts',(-0.0120149744006178,-0.138706589206355,
1.25424911570271));
#15560=CARTESIAN_POINT('Ctrl Pts',(0.110059129405696,-0.0852693704304675,
1.26219128382548));
#15561=CARTESIAN_POINT('Ctrl Pts',(0.13130776387206,0.0462833517151888,
1.27013345194827));
#15562=CARTESIAN_POINT('Ctrl Pts',(0.0322649968732001,0.135435768819968,
1.27807562007105));
#15563=CARTESIAN_POINT('Ctrl Pts',(-0.0881142830049797,0.102747609761224,
1.28551003991283));
#15564=CARTESIAN_POINT('Ctrl Pts',(-0.117534109666069,0.0315207854174475,
1.29029707038035));
#15565=CARTESIAN_POINT('Ctrl Pts',(-0.117823716245033,-0.000102811805890825,
1.29243671147362));
#15566=CARTESIAN_POINT('Origin',(0.,0.,-0.0924367114736175));
#15567=CARTESIAN_POINT('',(-0.117957988745754,-3.12301727557783E-5,1.18256328852638));
#15568=CARTESIAN_POINT('',(-0.117793553451004,0.000106755881474893,1.19243671147362));
#15569=CARTESIAN_POINT('',(-0.117775,2.85464118895969E-14,-0.0924367114736175));
#15570=CARTESIAN_POINT('Ctrl Pts',(-0.117957988745754,-3.12301727557569E-5,
1.18256328852638));
#15571=CARTESIAN_POINT('Ctrl Pts',(-0.117964007145535,-0.00173159226684161,
1.18267867767044));
#15572=CARTESIAN_POINT('Ctrl Pts',(-0.117160216762375,-0.0424221720604921,
1.1854403966936));
#15573=CARTESIAN_POINT('Ctrl Pts',(-0.0703321751825429,-0.12013338809653,
1.19084844559586));
#15574=CARTESIAN_POINT('Ctrl Pts',(0.0627954496153871,-0.124239193932754,
1.19878743523316));
#15575=CARTESIAN_POINT('Ctrl Pts',(0.138438143943654,-0.0146125323915816,
1.20672642487047));
#15576=CARTESIAN_POINT('Ctrl Pts',(0.0873502052771435,0.108390901091839,
1.21466541450777));
#15577=CARTESIAN_POINT('Ctrl Pts',(-0.043700859820065,0.132169893139269,
1.22260440414508));
#15578=CARTESIAN_POINT('Ctrl Pts',(-0.112119660921406,0.0591163174148552,
1.22857036215128));
#15579=CARTESIAN_POINT('Ctrl Pts',(-0.117839104743291,0.0100747194789664,
1.23188999027838));
#15580=CARTESIAN_POINT('Ctrl Pts',(-0.11774949833287,0.000107383800510997,
1.23256328852638));
#15581=CARTESIAN_POINT('Ctrl Pts',(-0.117793553451004,0.000106755881474891,
1.19243671147362));
#15582=CARTESIAN_POINT('Ctrl Pts',(-0.117510050331475,-0.0305433296418112,
1.19450912059683));
#15583=CARTESIAN_POINT('Ctrl Pts',(-0.0896091397727994,-0.100804620014092,
1.19922891909429));
#15584=CARTESIAN_POINT('Ctrl Pts',(0.0288222657999454,-0.136209964735594,
1.20659610696603));
#15585=CARTESIAN_POINT('Ctrl Pts',(0.130092623711363,-0.0495962373069701,
1.21453827508881));
#15586=CARTESIAN_POINT('Ctrl Pts',(0.112184773380136,0.082452738709893,
1.22248044321158));
#15587=CARTESIAN_POINT('Ctrl Pts',(-0.00849585454694533,0.138966535376798,
1.23042261133437));
#15588=CARTESIAN_POINT('Ctrl Pts',(-0.103054997843392,0.079672038485689,
1.23707470075504));
#15589=CARTESIAN_POINT('Ctrl Pts',(-0.11756927027536,0.0201573447738481,
1.24107940080146));
#15590=CARTESIAN_POINT('Ctrl Pts',(-0.117581795058195,-8.20683476789562E-6,
1.24243671147361));
#15591=CARTESIAN_POINT('Origin',(0.,0.,-0.0924367114736175));
#15592=CARTESIAN_POINT('',(-0.117657565919426,-8.78585414499747E-5,1.13256328852638));
#15593=CARTESIAN_POINT('',(-0.117937823388479,-5.4172489969917E-5,1.14243671147362));
#15594=CARTESIAN_POINT('',(-0.117775,2.85464118895969E-14,-0.0924367114736175));
#15595=CARTESIAN_POINT('Ctrl Pts',(-0.117657565919426,-8.78585414499974E-5,
1.13256328852638));
#15596=CARTESIAN_POINT('Ctrl Pts',(-0.11775046973706,-0.0134980674796043,
1.13346736506249));
#15597=CARTESIAN_POINT('Ctrl Pts',(-0.109441032251172,-0.0660497484721492,
1.13701777147771));
#15598=CARTESIAN_POINT('Ctrl Pts',(-0.0320511128216771,-0.13546723577438,
1.14321450777202));
#15599=CARTESIAN_POINT('Ctrl Pts',(0.0964380908528195,-0.100390938007982,
1.15115349740933));
#15600=CARTESIAN_POINT('Ctrl Pts',(0.136644831685568,0.0265863832644056,
1.15909248704664));
#15601=CARTESIAN_POINT('Ctrl Pts',(0.0517625939920979,0.129225692742072,
1.16703147668394));
#15602=CARTESIAN_POINT('Ctrl Pts',(-0.0785823129332351,0.113795317289389,
1.17485507717719));
#15603=CARTESIAN_POINT('Ctrl Pts',(-0.117825981412732,0.0372644419932696,
1.18003234779134));
#15604=CARTESIAN_POINT('Ctrl Pts',(-0.117957988745754,-3.12301727557569E-5,
1.18256328852638));
#15605=CARTESIAN_POINT('Ctrl Pts',(-0.117937823388479,-5.41724899699178E-5,
1.14243671147362));
#15606=CARTESIAN_POINT('Ctrl Pts',(-0.117955293269658,-0.0031110520517566,
1.14264406164367));
#15607=CARTESIAN_POINT('Ctrl Pts',(-0.116460933142332,-0.0451799670343263,
1.14549880118799));
#15608=CARTESIAN_POINT('Ctrl Pts',(-0.0660858892268601,-0.122541963197144,
1.15100093010657));
#15609=CARTESIAN_POINT('Ctrl Pts',(0.0671705316110708,-0.121950798202395,
1.15894309822935));
#15610=CARTESIAN_POINT('Ctrl Pts',(0.138891844802359,-0.00964017357273747,
1.16688526635212));
#15611=CARTESIAN_POINT('Ctrl Pts',(0.0833739592533277,0.111501840422208,
1.17482743447491));
#15612=CARTESIAN_POINT('Ctrl Pts',(-0.0485230383040216,0.130496713571114,
1.18276960259768));
#15613=CARTESIAN_POINT('Ctrl Pts',(-0.113150295826959,0.0561813708375219,
1.18863936159726));
#15614=CARTESIAN_POINT('Ctrl Pts',(-0.117872210070015,0.00861047923971886,
1.19186173122257));
#15615=CARTESIAN_POINT('Ctrl Pts',(-0.117793553451004,0.000106755881474891,
1.19243671147362));
#15616=CARTESIAN_POINT('Origin',(0.,0.,-0.0924367114736175));
#15617=CARTESIAN_POINT('',(-0.117641451221435,8.0229283111194E-5,1.08256328852638));
#15618=CARTESIAN_POINT('',(-0.117630591849015,-7.42484764288953E-5,1.09243671147362));
#15619=CARTESIAN_POINT('',(-0.117775,2.85464118895969E-14,-0.0924367114736175));
#15620=CARTESIAN_POINT('Ctrl Pts',(-0.117641451221435,8.02292831111745E-5,
1.08256328852638));
#15621=CARTESIAN_POINT('Ctrl Pts',(-0.117483998834985,-0.0250372639622414,
1.08425605245455));
#15622=CARTESIAN_POINT('Ctrl Pts',(-0.0972946570053161,-0.0896524615425008,
1.08859514626182));
#15623=CARTESIAN_POINT('Ctrl Pts',(0.00904258428980543,-0.13891320121148,
1.09558056994819));
#15624=CARTESIAN_POINT('Ctrl Pts',(0.121617839487272,-0.067732908692211,
1.1035195595855));
#15625=CARTESIAN_POINT('Ctrl Pts',(0.122860297649024,0.0654522196953821,
1.1114585492228));
#15626=CARTESIAN_POINT('Ctrl Pts',(0.0116325734791967,0.138720326685422,
1.11939753886011));
#15627=CARTESIAN_POINT('Ctrl Pts',(-0.096364912740844,0.0911171059582243,
1.1264324519613));
#15628=CARTESIAN_POINT('Ctrl Pts',(-0.117478530206868,0.0257550656131636,
1.13082103518339));
#15629=CARTESIAN_POINT('Ctrl Pts',(-0.117657565919426,-8.78585414499974E-5,
1.13256328852638));
#15630=CARTESIAN_POINT('Ctrl Pts',(-0.117630591849015,-7.42484764288814E-5,
1.09243671147362));
#15631=CARTESIAN_POINT('Ctrl Pts',(-0.117715241483118,-0.0147626739157663,
1.09342639206478));
#15632=CARTESIAN_POINT('Ctrl Pts',(-0.108350501834675,-0.0686384992808382,
1.0970634620302));
#15633=CARTESIAN_POINT('Ctrl Pts',(-0.0276126195379174,-0.136460326620484,
1.10334792136989));
#15634=CARTESIAN_POINT('Ctrl Pts',(0.0997182217817603,-0.0971604536002107,
1.11129008949267));
#15635=CARTESIAN_POINT('Ctrl Pts',(0.135696927507188,0.0311483765905046,
1.11923225761545));
#15636=CARTESIAN_POINT('Ctrl Pts',(0.0473633069609982,0.130922093830007,
1.12717442573822));
#15637=CARTESIAN_POINT('Ctrl Pts',(-0.0809210029008042,0.111284164335459,
1.13490924369095));
#15638=CARTESIAN_POINT('Ctrl Pts',(-0.117732242679493,0.0359183370635313,
1.13999667226941));
#15639=CARTESIAN_POINT('Ctrl Pts',(-0.117937823388479,-5.41724899699178E-5,
1.14243671147362));
#15640=CARTESIAN_POINT('Origin',(0.,0.,-0.0924367114736175));
#15641=CARTESIAN_POINT('',(-0.117948158721073,4.38502512853227E-5,1.03256328852638));
#15642=CARTESIAN_POINT('',(-0.117667547954054,9.20194976846214E-5,1.04243671147362));
#15643=CARTESIAN_POINT('',(-0.117775,2.85464118895969E-14,-0.0924367114736175));
#15644=CARTESIAN_POINT('Ctrl Pts',(-0.117948158721073,4.38502512853157E-5,
1.03256328852638));
#15645=CARTESIAN_POINT('Ctrl Pts',(-0.117773439871091,-0.0365306738650768,
1.03504473984661));
#15646=CARTESIAN_POINT('Ctrl Pts',(-0.0798690478914953,-0.112422454385097,
1.04017252104593));
#15647=CARTESIAN_POINT('Ctrl Pts',(0.0493427524230464,-0.130168884856471,
1.04794663212436));
#15648=CARTESIAN_POINT('Ctrl Pts',(0.136125055048066,-0.0291310004912345,
1.05588562176166));
#15649=CARTESIAN_POINT('Ctrl Pts',(0.0982941990358779,0.0985743183458784,
1.06382461139897));
#15650=CARTESIAN_POINT('Ctrl Pts',(-0.0295182596522469,0.136041604476578,
1.07176360103627));
#15651=CARTESIAN_POINT('Ctrl Pts',(-0.108818061611988,0.067537217334308,
1.07800982674541));
#15652=CARTESIAN_POINT('Ctrl Pts',(-0.11773014713001,0.0142293884972668,
1.08160972257545));
#15653=CARTESIAN_POINT('Ctrl Pts',(-0.117641451221435,8.02292831111745E-5,
1.08256328852638));
#15654=CARTESIAN_POINT('Ctrl Pts',(-0.117667547954054,9.20194976846197E-5,
1.04243671147362));
#15655=CARTESIAN_POINT('Ctrl Pts',(-0.117475882803567,-0.0261866690710452,
1.04420872248589));
#15656=CARTESIAN_POINT('Ctrl Pts',(-0.0957916308421219,-0.0920126959480487,
1.04862812287242));
#15657=CARTESIAN_POINT('Ctrl Pts',(0.0132451643780021,-0.13859452774087,
1.05569491263321));
#15658=CARTESIAN_POINT('Ctrl Pts',(0.123654649330263,-0.0639797248987874,
1.06363708075599));
#15659=CARTESIAN_POINT('Ctrl Pts',(0.120783771971213,0.0692470788374567,
1.07157924887876));
#15660=CARTESIAN_POINT('Ctrl Pts',(0.00726255089817806,0.139036444335888,
1.07952141700155));
#15661=CARTESIAN_POINT('Ctrl Pts',(-0.0979368667310299,0.0886295245336828,
1.08647390453316));
#15662=CARTESIAN_POINT('Ctrl Pts',(-0.117488804242801,0.0245287720112504,
1.09077900269052));
#15663=CARTESIAN_POINT('Ctrl Pts',(-0.117630591849015,-7.42484764288814E-5,
1.09243671147362));
#15664=CARTESIAN_POINT('Origin',(0.,0.,-0.0924367114736175));
#15665=CARTESIAN_POINT('',(-0.117771476475648,-0.000107683352847938,0.982563288526384));
#15666=CARTESIAN_POINT('',(-0.11796176292438,2.53781033017321E-5,0.992436711473616));
#15667=CARTESIAN_POINT('',(-0.117775,2.85464118895969E-14,-0.0924367114736175));
#15668=CARTESIAN_POINT('Ctrl Pts',(-0.117771476475648,-0.000107683352847945,
0.982563288526384));
#15669=CARTESIAN_POINT('Ctrl Pts',(-0.117856103358663,-0.00933799346614349,
0.983187097359559));
#15670=CARTESIAN_POINT('Ctrl Pts',(-0.112646870919438,-0.057630810124202,
0.986457236071836));
#15671=CARTESIAN_POINT('Ctrl Pts',(-0.0461590140787468,-0.131331607851033,
0.992373704663214));
#15672=CARTESIAN_POINT('Ctrl Pts',(0.0853128637208732,-0.110001641284132,
1.00031269430052));
#15673=CARTESIAN_POINT('Ctrl Pts',(0.138686661656432,0.0120272889735618,
1.00825168393783));
#15674=CARTESIAN_POINT('Ctrl Pts',(0.0651023256631918,0.123046060459907,
1.01619067357513));
#15675=CARTESIAN_POINT('Ctrl Pts',(-0.0680787277209358,0.121424596492465,
1.02412966321244));
#15676=CARTESIAN_POINT('Ctrl Pts',(-0.116790117880403,0.0438975063746073,
1.02958720152952));
#15677=CARTESIAN_POINT('Ctrl Pts',(-0.11795976781127,0.00247402277930658,
1.0323984099675));
#15678=CARTESIAN_POINT('Ctrl Pts',(-0.117948158721073,4.38502512853157E-5,
1.03256328852638));
#15679=CARTESIAN_POINT('Ctrl Pts',(-0.11796176292438,2.53781033017319E-5,
0.992436711473616));
#15680=CARTESIAN_POINT('Ctrl Pts',(-0.117851518882229,-0.0376119105440478,
0.994991052906992));
#15681=CARTESIAN_POINT('Ctrl Pts',(-0.077958511321084,-0.114458475672252,
1.00019278371463));
#15682=CARTESIAN_POINT('Ctrl Pts',(0.0529591494285269,-0.128760265574912,
1.00804190389653));
#15683=CARTESIAN_POINT('Ctrl Pts',(0.136912761112491,-0.0252739657289669,
1.0159840720193));
#15684=CARTESIAN_POINT('Ctrl Pts',(0.0954402180350474,0.101365883217864,
1.02392624014209));
#15685=CARTESIAN_POINT('Ctrl Pts',(-0.0334653697086341,0.135144169424284,
1.03186840826486));
#15686=CARTESIAN_POINT('Ctrl Pts',(-0.109792739119276,0.0652029671457737,
1.03803856537538));
#15687=CARTESIAN_POINT('Ctrl Pts',(-0.117762231070763,0.0130737646421874,
1.04156133311163));
#15688=CARTESIAN_POINT('Ctrl Pts',(-0.117667547954054,9.20194976846197E-5,
1.04243671147362));
#15689=CARTESIAN_POINT('Origin',(0.,0.,-0.0924367114736175));
#15690=CARTESIAN_POINT('',(-0.117585265278523,2.16484251076657E-5,0.932563288526384));
#15691=CARTESIAN_POINT('',(-0.117742563953077,-0.000107211314308964,0.942436711473616));
#15692=CARTESIAN_POINT('',(-0.117775,2.85464118895969E-14,-0.0924367114736175));
#15693=CARTESIAN_POINT('Ctrl Pts',(-0.117585265278523,2.16484251076635E-5,
0.932563288526384));
#15694=CARTESIAN_POINT('Ctrl Pts',(-0.117550805757046,-0.0209622679161363,
0.933975784751614));
#15695=CARTESIAN_POINT('Ctrl Pts',(-0.102172791552808,-0.0813069697478888,
0.938034610855947));
#15696=CARTESIAN_POINT('Ctrl Pts',(-0.00565790085648466,-0.139092177922979,
0.944739766839381));
#15697=CARTESIAN_POINT('Ctrl Pts',(0.113796373024222,-0.0801812402497705,
0.952678756476687));
#15698=CARTESIAN_POINT('Ctrl Pts',(0.129077866376032,0.0521301276928276,
0.960617746113992));
#15699=CARTESIAN_POINT('Ctrl Pts',(0.026197419344502,0.13671993644362,0.968556735751298));
#15700=CARTESIAN_POINT('Ctrl Pts',(-0.0906967139502387,0.0993396518733501,
0.975871916555428));
#15701=CARTESIAN_POINT('Ctrl Pts',(-0.117497098103867,0.02981894716558,
0.980540767480457));
#15702=CARTESIAN_POINT('Ctrl Pts',(-0.117771476475648,-0.000107683352847945,
0.982563288526384));
#15703=CARTESIAN_POINT('Ctrl Pts',(-0.117742563953077,-0.000107211314308957,
0.942436711473616));
#15704=CARTESIAN_POINT('Ctrl Pts',(-0.117833632602859,-0.0103126986533654,
0.943125993953839));
#15705=CARTESIAN_POINT('Ctrl Pts',(-0.111944766202914,-0.0596118697348184,
0.946462665808322));
#15706=CARTESIAN_POINT('Ctrl Pts',(-0.0428565117498991,-0.132465832952297,
0.952446727037066));
#15707=CARTESIAN_POINT('Ctrl Pts',(0.0880997963686447,-0.107806787258123,
0.960388895159846));
#15708=CARTESIAN_POINT('Ctrl Pts',(0.138347640177547,0.0156143509765511,
0.968331063282625));
#15709=CARTESIAN_POINT('Ctrl Pts',(0.061854832590724,0.124731139593481,
0.976273231405407));
#15710=CARTESIAN_POINT('Ctrl Pts',(-0.0713033562375951,0.119581390225944,
0.984215399528185));
#15711=CARTESIAN_POINT('Ctrl Pts',(-0.117322772537986,0.0417718924351975,
0.989603226217589));
#15712=CARTESIAN_POINT('Ctrl Pts',(-0.11796577882491,0.00139640554830399,
0.992343663532733));
#15713=CARTESIAN_POINT('Ctrl Pts',(-0.11796176292438,2.53781033017319E-5,
0.992436711473616));
#15714=CARTESIAN_POINT('Origin',(0.,0.,-0.0924367114736175));
#15715=CARTESIAN_POINT('',(-0.117850913371472,9.6525574830472E-5,0.882563288526384));
#15716=CARTESIAN_POINT('',(-0.117591231449503,3.54948526558943E-5,0.892436711473616));
#15717=CARTESIAN_POINT('',(-0.117775,2.85464118895969E-14,-0.0924367114736175));
#15718=CARTESIAN_POINT('Ctrl Pts',(-0.117850913371472,9.65255748304767E-5,
0.882563288526384));
#15719=CARTESIAN_POINT('Ctrl Pts',(-0.117563006813672,-0.0324172738354332,
0.884764472143669));
#15720=CARTESIAN_POINT('Ctrl Pts',(-0.0867151192651892,-0.104499852648429,
0.889611985640057));
#15721=CARTESIAN_POINT('Ctrl Pts',(0.0353397195745277,-0.134646760160997,
0.897105829015547));
#15722=CARTESIAN_POINT('Ctrl Pts',(0.132293719443212,-0.0433245611326863,
0.905044818652852));
#15723=CARTESIAN_POINT('Ctrl Pts',(0.108141885842356,0.0876583043865096,
0.912983808290157));
#15724=CARTESIAN_POINT('Ctrl Pts',(-0.0150064327997127,0.138395999855801,
0.920922797927463));
#15725=CARTESIAN_POINT('Ctrl Pts',(-0.104951114476159,0.0759553573435841,
0.927449291339539));
#15726=CARTESIAN_POINT('Ctrl Pts',(-0.117615366114572,0.01835136974357,
0.931329454872513));
#15727=CARTESIAN_POINT('Ctrl Pts',(-0.117585265278523,2.16484251076635E-5,
0.932563288526384));
#15728=CARTESIAN_POINT('Ctrl Pts',(-0.117591231449503,3.54948526559117E-5,
0.892436711473616));
#15729=CARTESIAN_POINT('Ctrl Pts',(-0.117532234588281,-0.0218238662162972,
0.893908324374946));
#15730=CARTESIAN_POINT('Ctrl Pts',(-0.101194437785642,-0.0830895288483654,
0.898027326650536));
#15731=CARTESIAN_POINT('Ctrl Pts',(-0.00250162451743248,-0.139203517821528,
0.904793718300386));
#15732=CARTESIAN_POINT('Ctrl Pts',(0.115632500949424,-0.0775435504945224,
0.912735886423165));
#15733=CARTESIAN_POINT('Ctrl Pts',(0.127835376168433,0.0551542754370876,
0.920678054545947));
#15734=CARTESIAN_POINT('Ctrl Pts',(0.0229279137899797,0.137325118854324,
0.928620222668725));
#15735=CARTESIAN_POINT('Ctrl Pts',(-0.0920562790907298,0.0974788594069619,
0.935873108311283));
#15736=CARTESIAN_POINT('Ctrl Pts',(-0.117483857027998,0.0288844367965532,
0.94047860457958));
#15737=CARTESIAN_POINT('Ctrl Pts',(-0.117742563953077,-0.000107211314308957,
0.942436711473616));
#15738=CARTESIAN_POINT('Origin',(0.,0.,-0.0924367114736175));
#15739=CARTESIAN_POINT('',(-0.11789232318732,-8.18790992476613E-5,0.832563288526384));
#15740=CARTESIAN_POINT('',(-0.117872825429845,8.99519344067963E-5,0.842436711473616));
#15741=CARTESIAN_POINT('',(-0.117775,2.85464118895969E-14,-0.0924367114736175));
#15742=CARTESIAN_POINT('Ctrl Pts',(-0.11789232318732,-8.18790992476734E-5,
0.832563288526384));
#15743=CARTESIAN_POINT('Ctrl Pts',(-0.117932494517479,-0.00515170743829337,
0.832906829656623));
#15744=CARTESIAN_POINT('Ctrl Pts',(-0.115332713682068,-0.0492334187378749,
0.835896700665964));
#15745=CARTESIAN_POINT('Ctrl Pts',(-0.059752088941783,-0.125731196083361,
0.841532901554406));
#15746=CARTESIAN_POINT('Ctrl Pts',(0.0732361146625898,-0.118385460722959,
0.849471891191712));
#15747=CARTESIAN_POINT('Ctrl Pts',(0.139181674492094,-0.00266594955618734,
0.857410880829018));
#15748=CARTESIAN_POINT('Ctrl Pts',(0.077715950067195,0.115494055719818,
0.865349870466323));
#15749=CARTESIAN_POINT('Ctrl Pts',(-0.0548934004223171,0.127927168308903,
0.87328886010363));
#15750=CARTESIAN_POINT('Ctrl Pts',(-0.114416768398411,0.0522742940766184,
0.879026666123649));
#15751=CARTESIAN_POINT('Ctrl Pts',(-0.117909136832228,0.0066718045071592,
0.882118142264567));
#15752=CARTESIAN_POINT('Ctrl Pts',(-0.117850913371472,9.65255748304767E-5,
0.882563288526384));
#15753=CARTESIAN_POINT('Ctrl Pts',(-0.117872825429845,8.99519344067998E-5,
0.842436711473616));
#15754=CARTESIAN_POINT('Ctrl Pts',(-0.117591169542271,-0.0331870933343037,
0.844690654796053));
#15755=CARTESIAN_POINT('Ctrl Pts',(-0.0854771005934613,-0.106025606004136,
0.84959198749275));
#15756=CARTESIAN_POINT('Ctrl Pts',(0.0380692928980519,-0.133920149482284,
0.857140709563706));
#15757=CARTESIAN_POINT('Ctrl Pts',(0.133179650076608,-0.0405839661022353,
0.865082877686486));
#15758=CARTESIAN_POINT('Ctrl Pts',(0.106283765719693,0.0899312995767124,
0.873025045809266));
#15759=CARTESIAN_POINT('Ctrl Pts',(-0.0179789669825735,0.138060255849953,
0.880967213932046));
#15760=CARTESIAN_POINT('Ctrl Pts',(-0.105798194743126,0.0742290978659706,
0.887437769153496));
#15761=CARTESIAN_POINT('Ctrl Pts',(-0.117638368248411,0.0175004969839459,
0.891260935000686));
#15762=CARTESIAN_POINT('Ctrl Pts',(-0.117591231449503,3.54948526559117E-5,
0.892436711473616));
#15763=CARTESIAN_POINT('Origin',(0.,0.,-0.0924367114736175));
#15764=CARTESIAN_POINT('',(-0.117598114366551,-4.51832715892789E-5,0.782563288526384));
#15765=CARTESIAN_POINT('',(-0.117874685330111,-8.92836445515327E-5,0.792436711473617));
#15766=CARTESIAN_POINT('',(-0.117775,2.85464118895969E-14,-0.0924367114736175));
#15767=CARTESIAN_POINT('Ctrl Pts',(-0.117598114366551,-4.518327158929E-5,
0.782563288526384));
#15768=CARTESIAN_POINT('Ctrl Pts',(-0.117656123976761,-0.0168608793038394,
0.783695517048678));
#15769=CARTESIAN_POINT('Ctrl Pts',(-0.106420815930739,-0.0729055463807818,
0.787474075450074));
#15770=CARTESIAN_POINT('Ctrl Pts',(-0.0202952816069424,-0.137719814645367,
0.793898963730571));
#15771=CARTESIAN_POINT('Ctrl Pts',(0.104705698854998,-0.0917352845351548,
0.801837953367879));
#15772=CARTESIAN_POINT('Ctrl Pts',(0.133855787965376,0.0382266115373486,
0.809776943005182));
#15773=CARTESIAN_POINT('Ctrl Pts',(0.0404700769297216,0.133194664588195,
0.81771593264249));
#15774=CARTESIAN_POINT('Ctrl Pts',(-0.0843190215395119,0.107398870964955,
0.825311381149555));
#15775=CARTESIAN_POINT('Ctrl Pts',(-0.117623050954756,0.0339016606582783,
0.830260499777521));
#15776=CARTESIAN_POINT('Ctrl Pts',(-0.11789232318732,-8.18790992476734E-5,
0.832563288526384));
#15777=CARTESIAN_POINT('Ctrl Pts',(-0.117874685330111,-8.9283644551537E-5,
0.792436711473617));
#15778=CARTESIAN_POINT('Ctrl Pts',(-0.11792303416021,-0.00583050672374999,
0.7928255958429));
#15779=CARTESIAN_POINT('Ctrl Pts',(-0.114931453360353,-0.0506053896743902,
0.795861869586443));
#15780=CARTESIAN_POINT('Ctrl Pts',(-0.0575513573065257,-0.126774282767806,
0.801545532704245));
#15781=CARTESIAN_POINT('Ctrl Pts',(0.0753527000357912,-0.117071978271622,
0.809487700827026));
#15782=CARTESIAN_POINT('Ctrl Pts',(0.139225942868322,-0.000119714417332432,
0.817429868949805));
#15783=CARTESIAN_POINT('Ctrl Pts',(0.0755539188089132,0.116942220141962,
0.825372037072586));
#15784=CARTESIAN_POINT('Ctrl Pts',(-0.0573332568284509,0.12687306712048,
0.833314205195366));
#15785=CARTESIAN_POINT('Ctrl Pts',(-0.114890414736801,0.0507419104293215,
0.839002429995709));
#15786=CARTESIAN_POINT('Ctrl Pts',(-0.117921990994851,0.00589875908008548,
0.842043265421793));
#15787=CARTESIAN_POINT('Ctrl Pts',(-0.117872825429845,8.99519344067998E-5,
0.842436711473616));
#15788=CARTESIAN_POINT('Origin',(0.,0.,-0.0924367114736175));
#15789=CARTESIAN_POINT('',(-0.11772691567491,0.000105512987197037,0.732563288526384));
#15790=CARTESIAN_POINT('',(-0.117591850253004,-3.65476421498312E-5,0.742436711473616));
#15791=CARTESIAN_POINT('',(-0.117775,2.85464118895969E-14,-0.0924367114736175));
#15792=CARTESIAN_POINT('Ctrl Pts',(-0.11772691567491,0.000105512987197042,
0.732563288526384));
#15793=CARTESIAN_POINT('Ctrl Pts',(-0.117479624464894,-0.0283451130369189,
0.734484204440733));
#15794=CARTESIAN_POINT('Ctrl Pts',(-0.0928318426870313,-0.096374559506161,
0.739051450234184));
#15795=CARTESIAN_POINT('Ctrl Pts',(0.0209425314183671,-0.137622876656644,
0.746265025906738));
#15796=CARTESIAN_POINT('Ctrl Pts',(0.126986869252672,-0.0570349089493802,
0.754204015544043));
#15797=CARTESIAN_POINT('Ctrl Pts',(0.11678343126468,0.0757646090434518,
0.762143005181349));
#15798=CARTESIAN_POINT('Ctrl Pts',(-0.000327234354877375,0.139206819944772,
0.770081994818654));
#15799=CARTESIAN_POINT('Ctrl Pts',(-0.100479183608201,0.0843410365921374,
0.776888755933667));
#15800=CARTESIAN_POINT('Ctrl Pts',(-0.117520539541507,0.0224420334666934,
0.781049187169576));
#15801=CARTESIAN_POINT('Ctrl Pts',(-0.117598114366551,-4.518327158929E-5,
0.782563288526384));
#15802=CARTESIAN_POINT('Ctrl Pts',(-0.117591850253004,-3.65476421498364E-5,
0.742436711473616));
#15803=CARTESIAN_POINT('Ctrl Pts',(-0.117640211257931,-0.0174335619022046,
0.743607926264006));
#15804=CARTESIAN_POINT('Ctrl Pts',(-0.105863856762799,-0.0740921523660566,
0.747426530428656));
#15805=CARTESIAN_POINT('Ctrl Pts',(-0.0182163644075178,-0.138029133036789,
0.753892523967566));
#15806=CARTESIAN_POINT('Ctrl Pts',(0.106128952536144,-0.0901139441634624,
0.761834692090347));
#15807=CARTESIAN_POINT('Ctrl Pts',(0.133249245915149,0.0403548753208232,
0.769776860213125));
#15808=CARTESIAN_POINT('Ctrl Pts',(0.0382995408207276,0.133854483197375,
0.777719028335907));
#15809=CARTESIAN_POINT('Ctrl Pts',(-0.0853693283863186,0.106155717082476,
0.785272312089402));
#15810=CARTESIAN_POINT('Ctrl Pts',(-0.117593892160246,0.0332537408718532,
0.79017820646864));
#15811=CARTESIAN_POINT('Ctrl Pts',(-0.117874685330111,-8.9283644551537E-5,
0.792436711473617));
#15812=CARTESIAN_POINT('Origin',(0.,0.,-0.0924367114736175));
#15813=CARTESIAN_POINT('',(-0.117964947617991,-1.73329198795185E-5,0.682563288526384));
#15814=CARTESIAN_POINT('',(-0.117740574064672,0.000107068518266168,0.692436711473616));
#15815=CARTESIAN_POINT('',(-0.117775,2.85464118895969E-14,-0.0924367114736175));
#15816=CARTESIAN_POINT('Ctrl Pts',(-0.117964947617991,-1.73329198795367E-5,
0.682563288526384));
#15817=CARTESIAN_POINT('Ctrl Pts',(-0.117966864156947,-0.000949576032666658,
0.682626561953687));
#15818=CARTESIAN_POINT('Ctrl Pts',(-0.117534558560489,-0.0408698671952461,
0.685336165260092));
#15819=CARTESIAN_POINT('Ctrl Pts',(-0.0726787294560835,-0.118728463672822,
0.690692098445597));
#15820=CARTESIAN_POINT('Ctrl Pts',(0.0603425395611779,-0.125448888878168,
0.698631088082904));
#15821=CARTESIAN_POINT('Ctrl Pts',(0.138124349154501,-0.0173294538893964,
0.706570077720209));
#15822=CARTESIAN_POINT('Ctrl Pts',(0.0894627833767505,0.106653908470079,
0.714509067357515));
#15823=CARTESIAN_POINT('Ctrl Pts',(-0.0410958292974484,0.133002927094911,
0.72244805699482));
#15824=CARTESIAN_POINT('Ctrl Pts',(-0.111546724107196,0.0606813038481789,
0.728466130717777));
#15825=CARTESIAN_POINT('Ctrl Pts',(-0.117820302634623,0.0108495967181263,
0.731837874561632));
#15826=CARTESIAN_POINT('Ctrl Pts',(-0.11772691567491,0.000105512987197042,
0.732563288526384));
#15827=CARTESIAN_POINT('Ctrl Pts',(-0.117740574064672,0.000107068518266165,
0.692436711473616));
#15828=CARTESIAN_POINT('Ctrl Pts',(-0.117483171888848,-0.0288182833237499,
0.694390256685113));
#15829=CARTESIAN_POINT('Ctrl Pts',(-0.0921515028359353,-0.0973455904149804,
0.698991191270869));
#15830=CARTESIAN_POINT('Ctrl Pts',(0.022691720100341,-0.137364345221032,
0.706239515230886));
#15831=CARTESIAN_POINT('Ctrl Pts',(0.127740337615313,-0.0553740340325759,
0.714181683353665));
#15832=CARTESIAN_POINT('Ctrl Pts',(0.115765682611161,0.077344581120379,
0.722123851476446));
#15833=CARTESIAN_POINT('Ctrl Pts',(-0.00226223072526165,0.139207614056346,
0.730066019599226));
#15834=CARTESIAN_POINT('Ctrl Pts',(-0.101117998472899,0.083225715609228,
0.736836972931616));
#15835=CARTESIAN_POINT('Ctrl Pts',(-0.117530897055598,0.0218902846491045,
0.740960536889746));
#15836=CARTESIAN_POINT('Ctrl Pts',(-0.117591850253004,-3.65476421498364E-5,
0.742436711473616));
#15837=CARTESIAN_POINT('Origin',(0.,0.,-0.0924367114736175));
#15838=CARTESIAN_POINT('',(-0.117676160015555,-9.46906955630148E-5,0.632563288526383));
#15839=CARTESIAN_POINT('',(-0.117962383120995,-2.41598447144192E-5,0.642436711473616));
#15840=CARTESIAN_POINT('',(-0.117775,2.85464118895969E-14,-0.0924367114736175));
#15841=CARTESIAN_POINT('Ctrl Pts',(-0.117676160015555,-9.46906955630045E-5,
0.632563288526383));
#15842=CARTESIAN_POINT('Ctrl Pts',(-0.117771520970562,-0.0127268345011372,
0.633415249345741));
#15843=CARTESIAN_POINT('Ctrl Pts',(-0.110078248258936,-0.064483421762156,
0.636913540044201));
#15844=CARTESIAN_POINT('Ctrl Pts',(-0.0347063025259737,-0.134811417789573,
0.643058160621763));
#15845=CARTESIAN_POINT('Ctrl Pts',(0.0944472082050275,-0.102266175560326,
0.65099715025907));
#15846=CARTESIAN_POINT('Ctrl Pts',(0.137140772714236,0.0238967416356601,
0.658936139896373));
#15847=CARTESIAN_POINT('Ctrl Pts',(0.054291358674537,0.128183829614862,
0.666875129533682));
#15848=CARTESIAN_POINT('Ctrl Pts',(-0.0772016597727435,0.11523146575827,
0.674750845743682));
#15849=CARTESIAN_POINT('Ctrl Pts',(-0.117886707375211,0.0380402955314478,
0.679980232074585));
#15850=CARTESIAN_POINT('Ctrl Pts',(-0.117964947617991,-1.73329198795367E-5,
0.682563288526384));
#15851=CARTESIAN_POINT('Ctrl Pts',(-0.117962383120995,-2.41598447144253E-5,
0.642436711473616));
#15852=CARTESIAN_POINT('Ctrl Pts',(-0.117966033213387,-0.0013279541977536,
0.642525197731959));
#15853=CARTESIAN_POINT('Ctrl Pts',(-0.117355585052125,-0.0416360146359673,
0.645261073364563));
#15854=CARTESIAN_POINT('Ctrl Pts',(-0.0715088964667609,-0.119458592094588,
0.650644338371427));
#15855=CARTESIAN_POINT('Ctrl Pts',(0.0616402393688536,-0.124837327709565,
0.658586506494205));
#15856=CARTESIAN_POINT('Ctrl Pts',(0.138320583400205,-0.0158522461166236,
0.666528674616987));
#15857=CARTESIAN_POINT('Ctrl Pts',(0.0882850628235238,0.107655121482266,
0.674470842739765));
#15858=CARTESIAN_POINT('Ctrl Pts',(-0.0426286451686149,0.132539337972556,
0.682413010862546));
#15859=CARTESIAN_POINT('Ctrl Pts',(-0.111894847147975,0.059748848130285,
0.68840163377383));
#15860=CARTESIAN_POINT('Ctrl Pts',(-0.117831996057943,0.0103805377030848,
0.691742867310853));
#15861=CARTESIAN_POINT('Ctrl Pts',(-0.117740574064672,0.000107068518266165,
0.692436711473616));
#15862=CARTESIAN_POINT('Origin',(0.,0.,-0.0924367114736175));
#15863=CARTESIAN_POINT('',(-0.117626285855324,7.11112359239178E-5,0.582563288526384));
#15864=CARTESIAN_POINT('',(-0.11766919235599,-9.26074537421634E-5,0.592436711473616));
#15865=CARTESIAN_POINT('',(-0.117775,2.85464118895969E-14,-0.0924367114736175));
#15866=CARTESIAN_POINT('Ctrl Pts',(-0.117626285855324,7.11112359239024E-5,
0.582563288526383));
#15867=CARTESIAN_POINT('Ctrl Pts',(-0.117492102008102,-0.0242809575267813,
0.584203936737797));
#15868=CARTESIAN_POINT('Ctrl Pts',(-0.0982512120079041,-0.0881067492982899,
0.588490914828312));
#15869=CARTESIAN_POINT('Ctrl Pts',(0.00631176444456456,-0.139064040754811,
0.595424222797929));
#15870=CARTESIAN_POINT('Ctrl Pts',(0.120263693490807,-0.0701091280034811,
0.603363212435234));
#15871=CARTESIAN_POINT('Ctrl Pts',(0.124122453355413,0.0630258865426945,
0.611302202072541));
#15872=CARTESIAN_POINT('Ctrl Pts',(0.0143556138404206,0.138465021405133,
0.619241191709845));
#15873=CARTESIAN_POINT('Ctrl Pts',(-0.0953630726970595,0.0926558297308384,
0.626328220527794));
#15874=CARTESIAN_POINT('Ctrl Pts',(-0.117475314221613,0.0265106736450616,
0.630768919466639));
#15875=CARTESIAN_POINT('Ctrl Pts',(-0.117676160015555,-9.46906955630045E-5,
0.632563288526383));
#15876=CARTESIAN_POINT('Ctrl Pts',(-0.11766919235599,-9.26074537421669E-5,
0.592436711473616));
#15877=CARTESIAN_POINT('Ctrl Pts',(-0.117764072896019,-0.0130062487266101,
0.593307528153066));
#15878=CARTESIAN_POINT('Ctrl Pts',(-0.109848366281979,-0.0650658641993071,
0.596825734206776));
#15879=CARTESIAN_POINT('Ctrl Pts',(-0.0336977294021144,-0.135086418755761,
0.602991329634746));
#15880=CARTESIAN_POINT('Ctrl Pts',(0.0952657566843092,-0.101529863106778,
0.610933497757526));
#15881=CARTESIAN_POINT('Ctrl Pts',(0.136956022624868,0.025038477707157,
0.618875665880307));
#15882=CARTESIAN_POINT('Ctrl Pts',(0.0531805018142573,0.128669000640787,
0.626817834003085));
#15883=CARTESIAN_POINT('Ctrl Pts',(-0.0778376600742765,0.114584191752874,
0.634671515867523));
#15884=CARTESIAN_POINT('Ctrl Pts',(-0.117856827377429,0.0376798124439797,
0.639877808357699));
#15885=CARTESIAN_POINT('Ctrl Pts',(-0.117962383120995,-2.41598447144253E-5,
0.642436711473616));
#15886=CARTESIAN_POINT('Origin',(0.,0.,-0.0924367114736175));
#15887=CARTESIAN_POINT('',(-0.117934829819181,5.63106208242181E-5,0.532563288526383));
#15888=CARTESIAN_POINT('',(-0.117629301205424,7.34277634442948E-5,0.542436711473615));
#15889=CARTESIAN_POINT('',(-0.117775,2.85464118895969E-14,-0.0924367114736175));
#15890=CARTESIAN_POINT('Ctrl Pts',(-0.117934829819181,5.63106208242166E-5,
0.532563288526383));
#15891=CARTESIAN_POINT('Ctrl Pts',(-0.117723349859012,-0.0357608023914865,
0.534992624129852));
#15892=CARTESIAN_POINT('Ctrl Pts',(-0.0811985738067347,-0.110967619805887,
0.540068289612422));
#15893=CARTESIAN_POINT('Ctrl Pts',(0.0467759446245483,-0.131113145053959,
0.547790284974095));
#15894=CARTESIAN_POINT('Ctrl Pts',(0.135526478334676,-0.031799677225719,
0.555729274611401));
#15895=CARTESIAN_POINT('Ctrl Pts',(0.100211809365564,0.0966242157284558,
0.563668264248707));
#15896=CARTESIAN_POINT('Ctrl Pts',(-0.0268399031138932,0.136595261273209,
0.571607253886012));
#15897=CARTESIAN_POINT('Ctrl Pts',(-0.108142973925314,0.0691035501437442,
0.577905595311905));
#15898=CARTESIAN_POINT('Ctrl Pts',(-0.117708537635025,0.0149983997031143,
0.581557606858695));
#15899=CARTESIAN_POINT('Ctrl Pts',(-0.117626285855324,7.11112359239024E-5,
0.582563288526383));
#15900=CARTESIAN_POINT('Ctrl Pts',(-0.117629301205424,7.34277634442983E-5,
0.542436711473615));
#15901=CARTESIAN_POINT('Ctrl Pts',(-0.11748956090956,-0.0244625652698295,
0.544089858574172));
#15902=CARTESIAN_POINT('Ctrl Pts',(-0.0980201725405651,-0.0884941619373469,
0.548390395048989));
#15903=CARTESIAN_POINT('Ctrl Pts',(0.00702343738442799,-0.139048728244533,
0.555338320898066));
#15904=CARTESIAN_POINT('Ctrl Pts',(0.12066450826877,-0.0694546898587181,
0.563280489020846));
#15905=CARTESIAN_POINT('Ctrl Pts',(0.123764493242992,0.063766979789076,
0.571222657143626));
#15906=CARTESIAN_POINT('Ctrl Pts',(0.0134834875971477,0.13857154491934,
0.579164825266405));
#15907=CARTESIAN_POINT('Ctrl Pts',(-0.0957036897026042,0.092147346049863,
0.586236176709736));
#15908=CARTESIAN_POINT('Ctrl Pts',(-0.117475624432153,0.0262528025703711,
0.590660138778806));
#15909=CARTESIAN_POINT('Ctrl Pts',(-0.11766919235599,-9.26074537421669E-5,
0.592436711473616));
#15910=CARTESIAN_POINT('Origin',(0.,0.,-0.0924367114736175));
#15911=CARTESIAN_POINT('',(-0.117794891956694,-0.000106411733115368,0.482563288526384));
#15912=CARTESIAN_POINT('',(-0.117936566864074,5.52347650140707E-5,0.492436711473616));
#15913=CARTESIAN_POINT('',(-0.117775,2.85464118895969E-14,-0.0924367114736175));
#15914=CARTESIAN_POINT('Ctrl Pts',(-0.117794891956694,-0.000106411733115381,
0.482563288526384));
#15915=CARTESIAN_POINT('Ctrl Pts',(-0.117872998614688,-0.00856127641466401,
0.483134981642805));
#15916=CARTESIAN_POINT('Ctrl Pts',(-0.113184542395844,-0.0560672187853419,
0.486353004638329));
#15917=CARTESIAN_POINT('Ctrl Pts',(-0.0487302328423073,-0.130399425645183,
0.492217357512954));
#15918=CARTESIAN_POINT('Ctrl Pts',(0.0831353173341669,-0.111656458896056,
0.50015634715026));
#15919=CARTESIAN_POINT('Ctrl Pts',(0.13889618212661,0.00930034365552528,
0.508095336787567));
#15920=CARTESIAN_POINT('Ctrl Pts',(0.0675071113591811,0.12174331898465,
0.516034326424871));
#15921=CARTESIAN_POINT('Ctrl Pts',(-0.0656800932930844,0.122738629397884,
0.523973316062178));
#15922=CARTESIAN_POINT('Ctrl Pts',(-0.116384786286051,0.04545243224792,
0.529482970096015));
#15923=CARTESIAN_POINT('Ctrl Pts',(-0.117953719733239,0.00325558390455253,
0.53234629425075));
#15924=CARTESIAN_POINT('Ctrl Pts',(-0.117934829819181,5.63106208242166E-5,
0.532563288526383));
#15925=CARTESIAN_POINT('Ctrl Pts',(-0.117936566864074,5.52347650140663E-5,
0.492436711473616));
#15926=CARTESIAN_POINT('Ctrl Pts',(-0.117728017843002,-0.0358510361847084,
0.494872188995279));
#15927=CARTESIAN_POINT('Ctrl Pts',(-0.0810366231971402,-0.111156550628637,
0.499955055891203));
#15928=CARTESIAN_POINT('Ctrl Pts',(0.0471380885036503,-0.131003351527116,
0.507685312161385));
#15929=CARTESIAN_POINT('Ctrl Pts',(0.135643160584381,-0.031381690295376,
0.515627480284167));
#15930=CARTESIAN_POINT('Ctrl Pts',(0.0998851624184703,0.0969888232104648,
0.523569648406945));
#15931=CARTESIAN_POINT('Ctrl Pts',(-0.0273779061153799,0.136507610615132,
0.531511816529727));
#15932=CARTESIAN_POINT('Ctrl Pts',(-0.108290992649607,0.0687756007668377,
0.537800837551949));
#15933=CARTESIAN_POINT('Ctrl Pts',(-0.117713344367368,0.0148299618267192,
0.541442469199912));
#15934=CARTESIAN_POINT('Ctrl Pts',(-0.117629301205424,7.34277634442983E-5,
0.542436711473615));
#15935=CARTESIAN_POINT('Origin',(0.,0.,-0.0924367114736175));
#15936=CARTESIAN_POINT('',(-0.117582256074849,9.06819982020624E-6,0.432563288526383));
#15937=CARTESIAN_POINT('',(-0.11779560903417,-0.000106574656651148,0.442436711473616));
#15938=CARTESIAN_POINT('',(-0.117775,2.85464118895969E-14,-0.0924367114736175));
#15939=CARTESIAN_POINT('Ctrl Pts',(-0.117582256074849,9.06819982019261E-6,
0.432563288526383));
#15940=CARTESIAN_POINT('Ctrl Pts',(-0.117568373935691,-0.020201912089319,
0.43392366903486));
#15941=CARTESIAN_POINT('Ctrl Pts',(-0.10300922874285,-0.0797477867736473,
0.437930379422439));
#15942=CARTESIAN_POINT('Ctrl Pts',(-0.00838939967687663,-0.138954178686792,
0.44458341968912));
#15943=CARTESIAN_POINT('Ctrl Pts',(0.11219917790857,-0.0824013973067221,
0.452522409326426));
#15944=CARTESIAN_POINT('Ctrl Pts',(0.13007709763057,0.0495842159710775,
0.460461398963732));
#15945=CARTESIAN_POINT('Ctrl Pts',(0.0288783492374893,0.136178877755608,
0.468400388601037));
#15946=CARTESIAN_POINT('Ctrl Pts',(-0.0895654556576369,0.100852400902523,
0.475767685121922));
#15947=CARTESIAN_POINT('Ctrl Pts',(-0.117511448025972,0.0305757367622385,
0.480488651763704));
#15948=CARTESIAN_POINT('Ctrl Pts',(-0.117794891956694,-0.000106411733115381,
0.482563288526384));
#15949=CARTESIAN_POINT('Ctrl Pts',(-0.11779560903417,-0.000106574656651151,
0.442436711473616));
#15950=CARTESIAN_POINT('Ctrl Pts',(-0.117873644338608,-0.00854245500997505,
0.443007130042126));
#15951=CARTESIAN_POINT('Ctrl Pts',(-0.113196618671047,-0.056044542179559,
0.446224937984896));
#15952=CARTESIAN_POINT('Ctrl Pts',(-0.0487473834415776,-0.130413074907061,
0.452090135301926));
#15953=CARTESIAN_POINT('Ctrl Pts',(0.0831820848081396,-0.111645054821459,
0.460032303424706));
#15954=CARTESIAN_POINT('Ctrl Pts',(0.138908217753341,0.00940130521287039,
0.467974471547486));
#15955=CARTESIAN_POINT('Ctrl Pts',(0.0673801526530663,0.121835103839429,
0.475916639670265));
#15956=CARTESIAN_POINT('Ctrl Pts',(-0.0658750545035054,0.12265543075329,
0.483858807793047));
#15957=CARTESIAN_POINT('Ctrl Pts',(-0.116424939330292,0.0453161125527027,
0.489365498394162));
#15958=CARTESIAN_POINT('Ctrl Pts',(-0.11795471279604,0.00317945345687678,
0.492224799621019));
#15959=CARTESIAN_POINT('Ctrl Pts',(-0.117936566864074,5.52347650140663E-5,
0.492436711473616));
#15960=CARTESIAN_POINT('Origin',(0.,0.,-0.0924367114736175));
#15961=CARTESIAN_POINT('',(-0.117828183671793,0.000101754196006455,0.382563288526383));
#15962=CARTESIAN_POINT('',(-0.117581664177921,7.09484545444172E-6,0.392436711473616));
#15963=CARTESIAN_POINT('',(-0.117775,2.85464118895969E-14,-0.0924367114736175));
#15964=CARTESIAN_POINT('Ctrl Pts',(-0.117828183671793,0.000101754196006446,
0.382563288526384));
#15965=CARTESIAN_POINT('Ctrl Pts',(-0.117538790254565,-0.0316580736410773,
0.384712356426916));
#15966=CARTESIAN_POINT('Ctrl Pts',(-0.0879068326507716,-0.103002379129266,
0.38950775420655));
#15967=CARTESIAN_POINT('Ctrl Pts',(0.0326876424682324,-0.135315053971568,
0.396949481865287));
#15968=CARTESIAN_POINT('Ctrl Pts',(0.13141703692502,-0.0459152284901983,
0.404888471502591));
#15969=CARTESIAN_POINT('Ctrl Pts',(0.109843140674695,0.0855168418978295,
0.412827461139898));
#15970=CARTESIAN_POINT('Ctrl Pts',(-0.0122846228212416,0.13866410438033,
0.420766450777203));
#15971=CARTESIAN_POINT('Ctrl Pts',(-0.104166535924894,0.0775181589932739,
0.427345059906032));
#15972=CARTESIAN_POINT('Ctrl Pts',(-0.117595378674006,0.0191142356295008,
0.431277339155758));
#15973=CARTESIAN_POINT('Ctrl Pts',(-0.117582256074849,9.06819982019261E-6,
0.432563288526383));
#15974=CARTESIAN_POINT('Ctrl Pts',(-0.117581664177921,7.09484545444172E-6,
0.392436711473616));
#15975=CARTESIAN_POINT('Ctrl Pts',(-0.117570873504463,-0.0200907396801347,
0.393789460463232));
#15976=CARTESIAN_POINT('Ctrl Pts',(-0.10312708440739,-0.079535468422451,
0.397789598827109));
#15977=CARTESIAN_POINT('Ctrl Pts',(-0.00873482453528946,-0.138951719454826,
0.404437126565246));
#15978=CARTESIAN_POINT('Ctrl Pts',(0.112042812448737,-0.0826455423945668,
0.412379294688026));
#15979=CARTESIAN_POINT('Ctrl Pts',(0.130177722634257,0.049372441998279,
0.420321462810806));
#15980=CARTESIAN_POINT('Ctrl Pts',(0.0290564652212241,0.136160197297018,
0.428263630933586));
#15981=CARTESIAN_POINT('Ctrl Pts',(-0.0895090212855029,0.100936776489487,
0.435635380487856));
#15982=CARTESIAN_POINT('Ctrl Pts',(-0.117511471984497,0.0306096014671689,
0.440359740667866));
#15983=CARTESIAN_POINT('Ctrl Pts',(-0.11779560903417,-0.000106574656651151,
0.442436711473616));
#15984=CARTESIAN_POINT('Origin',(0.,0.,-0.0924367114736175));
#15985=CARTESIAN_POINT('',(-0.117911328466355,-7.22474488887591E-5,0.332563288526384));
#15986=CARTESIAN_POINT('',(-0.117821685414254,0.000103165543095151,0.342436711473616));
#15987=CARTESIAN_POINT('',(-0.117775,2.85464118895969E-14,-0.0924367114736175));
#15988=CARTESIAN_POINT('Ctrl Pts',(-0.117911328466355,-7.22474488887752E-5,
0.332563288526384));
#15989=CARTESIAN_POINT('Ctrl Pts',(-0.117942332027964,-0.00437115939612809,
0.332854713939869));
#15990=CARTESIAN_POINT('Ctrl Pts',(-0.115777752883067,-0.0476754067323583,
0.335792469232457));
#15991=CARTESIAN_POINT('Ctrl Pts',(-0.0622106591311991,-0.12453304658572,
0.341376554404146));
#15992=CARTESIAN_POINT('Ctrl Pts',(0.0708961914151981,-0.119801401679107,
0.349315544041452));
#15993=CARTESIAN_POINT('Ctrl Pts',(0.1391024375543,-0.00539978406154301,
0.357254533678757));
#15994=CARTESIAN_POINT('Ctrl Pts',(0.0799699354250877,0.113944965792994,
0.365193523316063));
#15995=CARTESIAN_POINT('Ctrl Pts',(-0.0523695618881846,0.128980908622551,
0.373132512953369));
#15996=CARTESIAN_POINT('Ctrl Pts',(-0.113921748517257,0.0538356345748906,
0.378922434690143));
#15997=CARTESIAN_POINT('Ctrl Pts',(-0.117895144954496,0.00745050051778832,
0.382066026547814));
#15998=CARTESIAN_POINT('Ctrl Pts',(-0.117828183671793,0.000101754196006446,
0.382563288526384));
#15999=CARTESIAN_POINT('Ctrl Pts',(-0.117821685414254,0.000103165543095145,
0.342436711473616));
#16000=CARTESIAN_POINT('Ctrl Pts',(-0.117532262555972,-0.0314544122979593,
0.344571790884339));
#16001=CARTESIAN_POINT('Ctrl Pts',(-0.0882170202347594,-0.102616110661261,
0.349354259669323));
#16002=CARTESIAN_POINT('Ctrl Pts',(0.0320320385160992,-0.135491055083419,
0.356784117828566));
#16003=CARTESIAN_POINT('Ctrl Pts',(0.131227975626944,-0.0465090949381858,
0.364726285951346));
#16004=CARTESIAN_POINT('Ctrl Pts',(0.110205605501345,0.0850799742312894,
0.372668454074126));
#16005=CARTESIAN_POINT('Ctrl Pts',(-0.0117764211155082,0.138727046407055,
0.380610622196906));
#16006=CARTESIAN_POINT('Ctrl Pts',(-0.10403099481448,0.0777947493501838,
0.387200041330069));
#16007=CARTESIAN_POINT('Ctrl Pts',(-0.117591991327853,0.019241607989002,
0.391142071088973));
#16008=CARTESIAN_POINT('Ctrl Pts',(-0.117581664177921,7.09484545444172E-6,
0.392436711473616));
#16009=CARTESIAN_POINT('Origin',(0.,0.,-0.0924367114736175));
#16010=CARTESIAN_POINT('',(-0.117608153246896,-5.64262068778628E-5,0.282563288526383));
#16011=CARTESIAN_POINT('',(-0.117918861549493,-6.80329776671096E-5,0.292436711473615));
#16012=CARTESIAN_POINT('',(-0.117775,2.85464118895969E-14,-0.0924367114736175));
#16013=CARTESIAN_POINT('Ctrl Pts',(-0.117608153246896,-5.64262068778604E-5,
0.282563288526383));
#16014=CARTESIAN_POINT('Ctrl Pts',(-0.117677606263852,-0.0160946837114709,
0.283643401331924));
#16015=CARTESIAN_POINT('Ctrl Pts',(-0.107144424846824,-0.0713401098021974,
0.287369844016567));
#16016=CARTESIAN_POINT('Ctrl Pts',(-0.0229969941138309,-0.137294515779738,
0.293742616580312));
#16017=CARTESIAN_POINT('Ctrl Pts',(0.102883268653204,-0.0937746172089793,
0.301681606217617));
#16018=CARTESIAN_POINT('Ctrl Pts',(0.134580950019115,0.0355895166223291,
0.309620595854923));
#16019=CARTESIAN_POINT('Ctrl Pts',(0.0430789950773988,0.13237388709478,
0.317559585492229));
#16020=CARTESIAN_POINT('Ctrl Pts',(-0.0830523456774332,0.10887452531409,
0.325207149716049));
#16021=CARTESIAN_POINT('Ctrl Pts',(-0.11766079978112,0.0346657214219864,
0.330208384060767));
#16022=CARTESIAN_POINT('Ctrl Pts',(-0.117911328466355,-7.22474488887752E-5,
0.332563288526384));
#16023=CARTESIAN_POINT('Ctrl Pts',(-0.117918861549493,-6.80329776671157E-5,
0.292436711473616));
#16024=CARTESIAN_POINT('Ctrl Pts',(-0.117946256357307,-0.00405052459867665,
0.292706731931186));
#16025=CARTESIAN_POINT('Ctrl Pts',(-0.11595553950755,-0.0470512577090033,
0.295624141763016));
#16026=CARTESIAN_POINT('Ctrl Pts',(-0.0631725212350128,-0.124068972994571,
0.301188940969106));
#16027=CARTESIAN_POINT('Ctrl Pts',(0.0700327441786229,-0.12032993078169,
0.309131109091886));
#16028=CARTESIAN_POINT('Ctrl Pts',(0.139080821187468,-0.00635631000930847,
0.317073277214666));
#16029=CARTESIAN_POINT('Ctrl Pts',(0.0807165776729536,0.11344034374014,
0.325015445337446));
#16030=CARTESIAN_POINT('Ctrl Pts',(-0.0515923433190751,0.129313988454311,
0.332957613460226));
#16031=CARTESIAN_POINT('Ctrl Pts',(-0.113774867115171,0.0543021652640841,
0.338764702172283));
#16032=CARTESIAN_POINT('Ctrl Pts',(-0.117891132111753,0.00767537174388221,
0.341924401510079));
#16033=CARTESIAN_POINT('Ctrl Pts',(-0.117821685414254,0.000103165543095145,
0.342436711473616));
#16034=CARTESIAN_POINT('Origin',(0.,0.,-0.0924367114736175));
#16035=CARTESIAN_POINT('',(-0.117705188630573,0.000102098618198066,0.232563288526383));
#16036=CARTESIAN_POINT('',(-0.1176142238744,-6.23262858038681E-5,0.242436711473616));
#16037=CARTESIAN_POINT('',(-0.117775,2.85464118895969E-14,-0.0924367114736175));
#16038=CARTESIAN_POINT('Ctrl Pts',(-0.117705188630573,0.000102098618198071,
0.232563288526383));
#16039=CARTESIAN_POINT('Ctrl Pts',(-0.117475649963863,-0.0275896003179174,
0.234432088723979));
#16040=CARTESIAN_POINT('Ctrl Pts',(-0.0938913217252411,-0.0948462909608301,
0.238947218800678));
#16041=CARTESIAN_POINT('Ctrl Pts',(0.0182347644767634,-0.138007750384372,
0.246108678756477));
#16042=CARTESIAN_POINT('Ctrl Pts',(0.125841858853055,-0.0595186723796334,
0.254047668393783));
#16043=CARTESIAN_POINT('Ctrl Pts',(0.118249355954961,0.073455671106145,
0.261986658031089));
#16044=CARTESIAN_POINT('Ctrl Pts',(0.00240767183786234,0.139186381940956,
0.269925647668394));
#16045=CARTESIAN_POINT('Ctrl Pts',(-0.0995777503027144,0.0858938305448248,
0.27678452450016));
#16046=CARTESIAN_POINT('Ctrl Pts',(-0.117507442931816,0.0231998416616275,
0.280997071452822));
#16047=CARTESIAN_POINT('Ctrl Pts',(-0.117608153246896,-5.64262068778604E-5,
0.282563288526383));
#16048=CARTESIAN_POINT('Ctrl Pts',(-0.1176142238744,-6.2326285803882E-5,
0.242436711473616));
#16049=CARTESIAN_POINT('Ctrl Pts',(-0.117689148257971,-0.0156863246439697,
0.243489062352292));
#16050=CARTESIAN_POINT('Ctrl Pts',(-0.107519643382358,-0.0705218816827611,
0.247188802605229));
#16051=CARTESIAN_POINT('Ctrl Pts',(-0.024381182195918,-0.137074561658528,
0.253535932232426));
#16052=CARTESIAN_POINT('Ctrl Pts',(0.101985705091022,-0.094777599970642,
0.261478100355206));
#16053=CARTESIAN_POINT('Ctrl Pts',(0.134923209124943,0.0343453801629359,
0.269420268477986));
#16054=CARTESIAN_POINT('Ctrl Pts',(0.0442571924125319,0.132004463632409,
0.277362436600766));
#16055=CARTESIAN_POINT('Ctrl Pts',(-0.0824920331482911,0.109525057495754,
0.285034584265976));
#16056=CARTESIAN_POINT('Ctrl Pts',(-0.117677666622401,0.0349954280503056,
0.290059342556926));
#16057=CARTESIAN_POINT('Ctrl Pts',(-0.117918861549493,-6.80329776671157E-5,
0.292436711473616));
#16058=CARTESIAN_POINT('Origin',(0.,0.,-0.0924367114736175));
#16059=CARTESIAN_POINT('',(-0.117967994073432,-3.0724305424694E-6,0.182563288526383));
#16060=CARTESIAN_POINT('',(-0.117691121003631,9.91971943564221E-5,0.192436711473615));
#16061=CARTESIAN_POINT('',(-0.117775,2.85464118895969E-14,-0.0924367114736175));
#16062=CARTESIAN_POINT('Ctrl Pts',(-0.117967994073432,-3.07243054247449E-6,
0.182563288526383));
#16063=CARTESIAN_POINT('Ctrl Pts',(-0.117968057042159,-0.000167453844217198,
0.182574446236933));
#16064=CARTESIAN_POINT('Ctrl Pts',(-0.117893299674953,-0.0393189363008842,
0.185231933826584));
#16065=CARTESIAN_POINT('Ctrl Pts',(-0.0749972298318695,-0.11727771015962,
0.190535751295337));
#16066=CARTESIAN_POINT('Ctrl Pts',(0.0578663373665801,-0.126610160769685,
0.198474740932643));
#16067=CARTESIAN_POINT('Ctrl Pts',(0.13775723856723,-0.0200396862227523,
0.206413730569949));
#16068=CARTESIAN_POINT('Ctrl Pts',(0.091540828968026,0.104875747581476,
0.214352720207254));
#16069=CARTESIAN_POINT('Ctrl Pts',(-0.0384749358425138,0.133784622116252,
0.22229170984456));
#16070=CARTESIAN_POINT('Ctrl Pts',(-0.110955338697302,0.0622468391270206,
0.22836189928427));
#16071=CARTESIAN_POINT('Ctrl Pts',(-0.11780069007939,0.0116234575531164,
0.231785758844877));
#16072=CARTESIAN_POINT('Ctrl Pts',(-0.117705188630573,0.000102098618198071,
0.232563288526383));
#16073=CARTESIAN_POINT('Ctrl Pts',(-0.117691121003631,9.91971943564221E-5,
0.192436711473615));
#16074=CARTESIAN_POINT('Ctrl Pts',(-0.117474218986382,-0.0270951350261672,
0.194271392773399));
#16075=CARTESIAN_POINT('Ctrl Pts',(-0.0945676524372527,-0.0938598508209937,
0.198753463447442));
#16076=CARTESIAN_POINT('Ctrl Pts',(0.0165156171993534,-0.138242945169174,
0.205882923495746));
#16077=CARTESIAN_POINT('Ctrl Pts',(0.125131592687617,-0.061040658666823,
0.213825091618526));
#16078=CARTESIAN_POINT('Ctrl Pts',(0.119114174013628,0.0720811421096423,
0.221767259741306));
#16079=CARTESIAN_POINT('Ctrl Pts',(0.0039759348809324,0.139169211541763,
0.229709427864086));
#16080=CARTESIAN_POINT('Ctrl Pts',(-0.0990660356104632,0.0867677816679632,
0.236599245108189));
#16081=CARTESIAN_POINT('Ctrl Pts',(-0.117500661679058,0.0236188235484957,
0.240841672978032));
#16082=CARTESIAN_POINT('Ctrl Pts',(-0.1176142238744,-6.2326285803882E-5,
0.242436711473616));
#16083=CARTESIAN_POINT('Origin',(0.,0.,-0.0924367114736175));
#16084=CARTESIAN_POINT('',(-0.117696212882312,-0.000100181105204699,0.132563288526383));
#16085=CARTESIAN_POINT('',(-0.117967699956222,8.3697257429456E-6,0.142436711473616));
#16086=CARTESIAN_POINT('',(-0.117775,2.85464118895969E-14,-0.0924367114736175));
#16087=CARTESIAN_POINT('Ctrl Pts',(-0.117696212882312,-0.000100181105204706,
0.132563288526383));
#16088=CARTESIAN_POINT('Ctrl Pts',(-0.117792074781153,-0.0119544960022407,
0.133363133628988));
#16089=CARTESIAN_POINT('Ctrl Pts',(-0.110696412003459,-0.0629173266909915,
0.136809308610694));
#16090=CARTESIAN_POINT('Ctrl Pts',(-0.0373480950846616,-0.134103559412242,
0.142901813471503));
#16091=CARTESIAN_POINT('Ctrl Pts',(0.0924198687735613,-0.104101940294199,
0.150840803108809));
#16092=CARTESIAN_POINT('Ctrl Pts',(0.137583777756591,0.0211978768359354,
0.158779792746114));
#16093=CARTESIAN_POINT('Ctrl Pts',(0.0567991668878991,0.127092487218924,
0.16671878238342));
#16094=CARTESIAN_POINT('Ctrl Pts',(-0.0757945745091616,0.116657324056303,
0.174646614310176));
#16095=CARTESIAN_POINT('Ctrl Pts',(-0.117953122434976,0.0388197061692436,
0.179928116357831));
#16096=CARTESIAN_POINT('Ctrl Pts',(-0.117967994073432,-3.07243054247449E-6,
0.182563288526383));
#16097=CARTESIAN_POINT('Ctrl Pts',(-0.117967699956222,8.3697257429579E-6,
0.142436711473616));
#16098=CARTESIAN_POINT('Ctrl Pts',(-0.117928252023989,-0.038547130539091,
0.145053723194506));
#16099=CARTESIAN_POINT('Ctrl Pts',(-0.0762804946418446,-0.116178754198862,
0.150318124289656));
#16100=CARTESIAN_POINT('Ctrl Pts',(0.0559861945572589,-0.127473226882309,
0.158229914759066));
#16101=CARTESIAN_POINT('Ctrl Pts',(0.137471621702818,-0.0220324926503626,
0.166172082881846));
#16102=CARTESIAN_POINT('Ctrl Pts',(0.0930189202108026,0.103592267873211,
0.174114251004626));
#16103=CARTESIAN_POINT('Ctrl Pts',(-0.0366486683060043,0.134315868829211,
0.182056419127406));
#16104=CARTESIAN_POINT('Ctrl Pts',(-0.110544190454925,0.0633195416932908,
0.188163905950403));
#16105=CARTESIAN_POINT('Ctrl Pts',(-0.11778720200735,0.0121454601492482,
0.191624003399139));
#16106=CARTESIAN_POINT('Ctrl Pts',(-0.117691121003631,9.91971943564221E-5,
0.192436711473615));
#16107=CARTESIAN_POINT('Origin',(0.,0.,-0.0924367114736175));
#16108=CARTESIAN_POINT('',(-0.117613109409711,6.11591708146705E-5,0.0825632885263832));
#16109=CARTESIAN_POINT('',(-0.117715749944134,-0.000104199409386274,0.0924367114736155));
#16110=CARTESIAN_POINT('',(-0.117775,2.85464118895969E-14,-0.0924367114736175));
#16111=CARTESIAN_POINT('Ctrl Pts',(-0.117613109409711,6.11591708146765E-5,
0.0825632885263832));
#16112=CARTESIAN_POINT('Ctrl Pts',(-0.117502393620717,-0.0235240259785673,
0.0841518210210431));
#16113=CARTESIAN_POINT('Ctrl Pts',(-0.0991849320095013,-0.0865581493706475,
0.088386683394805));
#16114=CARTESIAN_POINT('Ctrl Pts',(0.00357853460314598,-0.139161043603659,
0.0952678756476685));
#16115=CARTESIAN_POINT('Ctrl Pts',(0.118863112008681,-0.0724583686054966,
0.103206865284975));
#16116=CARTESIAN_POINT('Ctrl Pts',(0.125336705278751,0.0605752693714656,
0.11114585492228));
#16117=CARTESIAN_POINT('Ctrl Pts',(0.0170731091066207,0.138156245709763,
0.119084844559586));
#16118=CARTESIAN_POINT('Ctrl Pts',(-0.094337657277608,0.0941904991302726,
0.126223989094287));
#16119=CARTESIAN_POINT('Ctrl Pts',(-0.11747491061231,0.0272661325996615,
0.130716803749886));
#16120=CARTESIAN_POINT('Ctrl Pts',(-0.117696212882312,-0.000100181105204706,
0.132563288526383));
#16121=CARTESIAN_POINT('Ctrl Pts',(-0.117715749944134,-0.000104199409386274,
0.0924367114736155));
#16122=CARTESIAN_POINT('Ctrl Pts',(-0.117810584636384,-0.011244028442556,
0.0931886642413524));
#16123=CARTESIAN_POINT('Ctrl Pts',(-0.111246641208053,-0.0614941526881817,
0.0965880063833492));
#16124=CARTESIAN_POINT('Ctrl Pts',(-0.0397151780004399,-0.133441281507892,
0.102634737899606));
#16125=CARTESIAN_POINT('Ctrl Pts',(0.0906220264938673,-0.105695447092796,
0.110576906022386));
#16126=CARTESIAN_POINT('Ctrl Pts',(0.137940159127448,0.0188783162799928,
0.118519074145166));
#16127=CARTESIAN_POINT('Ctrl Pts',(0.0588909273047484,0.126157580947307,
0.126461242267946));
#16128=CARTESIAN_POINT('Ctrl Pts',(-0.074108440039672,0.117863552156501,
0.134403410390726));
#16129=CARTESIAN_POINT('Ctrl Pts',(-0.117763087033452,0.0399060678969832,
0.139728566792616));
#16130=CARTESIAN_POINT('Ctrl Pts',(-0.117968157858494,0.000455912857932787,
0.142406333820246));
#16131=CARTESIAN_POINT('Ctrl Pts',(-0.117967699956222,8.3697257429579E-6,
0.142436711473616));
#16132=CARTESIAN_POINT('Origin',(0.,0.,-0.0924367114736175));
#16133=CARTESIAN_POINT('',(-0.117917485785546,7.60014832213593E-5,0.0325632885263832));
#16134=CARTESIAN_POINT('',(-0.117600989619072,5.04992496179954E-5,0.0424367114736154));
#16135=CARTESIAN_POINT('',(-0.117775,2.85464118895969E-14,-0.0924367114736175));
#16136=CARTESIAN_POINT('Ctrl Pts',(-0.117917485785546,7.60014832213644E-5,
0.0325632885263832));
#16137=CARTESIAN_POINT('Ctrl Pts',(-0.117676727567847,-0.0349830640657269,
0.0349405084130983));
#16138=CARTESIAN_POINT('Ctrl Pts',(-0.0825043195215805,-0.109517225708346,
0.0399640581789154));
#16139=CARTESIAN_POINT('Ctrl Pts',(0.0441923146003338,-0.131999388615902,
0.0476339378238343));
#16140=CARTESIAN_POINT('Ctrl Pts',(0.134874939024977,-0.034459980695041,
0.0555729274611401));
#16141=CARTESIAN_POINT('Ctrl Pts',(0.102091080224759,0.094638871230671,
0.0635119170984456));
#16142=CARTESIAN_POINT('Ctrl Pts',(-0.0241513666277066,0.137095110112719,
0.0714509067357516));
#16143=CARTESIAN_POINT('Ctrl Pts',(-0.107448046275642,0.0706698818446754,
0.0778013638783972));
#16144=CARTESIAN_POINT('Ctrl Pts',(-0.117686834607281,0.0157664388843013,
0.0815054911419412));
#16145=CARTESIAN_POINT('Ctrl Pts',(-0.117613109409711,6.11591708146765E-5,
0.0825632885263832));
#16146=CARTESIAN_POINT('Ctrl Pts',(-0.117600989619072,5.04992496179954E-5,
0.0424367114736154));
#16147=CARTESIAN_POINT('Ctrl Pts',(-0.117514779739531,-0.0227353060542692,
0.043970994662459));
#16148=CARTESIAN_POINT('Ctrl Pts',(-0.100129952091853,-0.0849605109884783,
0.0481526672255625));
#16149=CARTESIAN_POINT('Ctrl Pts',(0.000787973702835166,-0.139222729671589,
0.054981729162926));
#16150=CARTESIAN_POINT('Ctrl Pts',(0.117431922513572,-0.0747907597173192,
0.0629238972857061));
#16151=CARTESIAN_POINT('Ctrl Pts',(0.126496838785129,0.0581591461343325,
0.070866065408486));
#16152=CARTESIAN_POINT('Ctrl Pts',(0.0196773008918215,0.137828289815661,
0.0788082335312661));
#16153=CARTESIAN_POINT('Ctrl Pts',(-0.0933482651079043,0.0956446566614129,
0.085998448886309));
#16154=CARTESIAN_POINT('Ctrl Pts',(-0.11747670148927,0.0279758085988667,
0.0905412748670923));
#16155=CARTESIAN_POINT('Ctrl Pts',(-0.117715749944134,-0.000104199409386274,
0.0924367114736155));
#16156=CARTESIAN_POINT('Origin',(0.,0.,1.55));
#16157=CARTESIAN_POINT('',(-0.143211704627722,-5.70397197726547E-6,1.50700023576178));
#16158=CARTESIAN_POINT('Ctrl Pts',(-0.0334019664626774,0.112939183906323,
1.532225));
#16159=CARTESIAN_POINT('Ctrl Pts',(-0.0250606930336426,0.115799676338094,
1.53184761307169));
#16160=CARTESIAN_POINT('Ctrl Pts',(-0.0164287086124659,0.117635554524944,
1.53147359869818));
#16161=CARTESIAN_POINT('Ctrl Pts',(-0.00767226928320402,0.118510614220874,
1.53110056493424));
#16162=CARTESIAN_POINT('Ctrl Pts',(-0.0042150196872779,0.118856108509867,
1.53095328237096));
#16163=CARTESIAN_POINT('Ctrl Pts',(-0.000736351480830917,0.119051293525916,
1.53080607672538));
#16164=CARTESIAN_POINT('Ctrl Pts',(0.00274830211697625,0.119097943881266,
1.53065904037218));
#16165=CARTESIAN_POINT('Ctrl Pts',(0.00972321854123044,0.119191319684798,
1.53036473098213));
#16166=CARTESIAN_POINT('Ctrl Pts',(0.0166907125456733,0.118690968429664,
1.53007241075126));
#16167=CARTESIAN_POINT('Ctrl Pts',(0.0235721318645625,0.11762150546261,
1.52978094357425));
#16168=CARTESIAN_POINT('Ctrl Pts',(0.0273478463565568,0.117034709826966,
1.52962102062912));
#16169=CARTESIAN_POINT('Ctrl Pts',(0.0310977188904398,0.116276259986281,
1.52946135449799));
#16170=CARTESIAN_POINT('Ctrl Pts',(0.0348087249896146,0.115347945392283,
1.52930175751644));
#16171=CARTESIAN_POINT('Ctrl Pts',(0.0378768737129624,0.114580442682688,
1.52916980751093));
#16172=CARTESIAN_POINT('Ctrl Pts',(0.0409182562642153,0.113696477767379,
1.52903790896105));
#16173=CARTESIAN_POINT('Ctrl Pts',(0.0439120268522727,0.112701821307647,
1.52890655030309));
#16174=CARTESIAN_POINT('Ctrl Pts',(0.0504861734289241,0.110517613410832,
1.52861809430882));
#16175=CARTESIAN_POINT('Ctrl Pts',(0.0568477403450367,0.107796947733889,
1.528331525126));
#16176=CARTESIAN_POINT('Ctrl Pts',(0.0629211062797432,0.10455513280498,
1.52804576869741));
#16177=CARTESIAN_POINT('Ctrl Pts',(0.0667529140263229,0.102509807084265,
1.52786547926507));
#16178=CARTESIAN_POINT('Ctrl Pts',(0.0704699809867569,0.100256700264741,
1.52768551335768));
#16179=CARTESIAN_POINT('Ctrl Pts',(0.0740519796445933,0.0977963961590643,
1.52750560123222));
#16180=CARTESIAN_POINT('Ctrl Pts',(0.0761474027326905,0.0963571499395001,
1.52740035495562));
#16181=CARTESIAN_POINT('Ctrl Pts',(0.0781972522873126,0.0948464165467323,
1.52729509152825));
#16182=CARTESIAN_POINT('Ctrl Pts',(0.0801950758490376,0.0932655888959708,
1.52718986717129));
#16183=CARTESIAN_POINT('Ctrl Pts',(0.0872135629190184,0.0877120362002772,
1.52682020700562));
#16184=CARTESIAN_POINT('Ctrl Pts',(0.0935342345834078,0.0813437113039547,
1.52645409167081));
#16185=CARTESIAN_POINT('Ctrl Pts',(0.0991216768718319,0.0743433873765979,
1.52608928877518));
#16186=CARTESIAN_POINT('Ctrl Pts',(0.101857856375295,0.0709153174549959,
1.52591064420861));
#16187=CARTESIAN_POINT('Ctrl Pts',(0.104417791592617,0.0673349702414553,
1.52573231437502));
#16188=CARTESIAN_POINT('Ctrl Pts',(0.106794530290299,0.0636205708890664,
1.52555403711528));
#16189=CARTESIAN_POINT('Ctrl Pts',(0.108394385735532,0.0611202951812291,
1.52543403324399));
#16190=CARTESIAN_POINT('Ctrl Pts',(0.109912312880749,0.0585571637778213,
1.52531395827658));
#16191=CARTESIAN_POINT('Ctrl Pts',(0.111341951189028,0.0559432008961949,
1.5251940432238));
#16192=CARTESIAN_POINT('Ctrl Pts',(0.115894033640165,0.0476201345006791,
1.52481222412716));
#16193=CARTESIAN_POINT('Ctrl Pts',(0.119530893641226,0.0388304356906876,
1.52443409356659));
#16194=CARTESIAN_POINT('Ctrl Pts',(0.122195159250079,0.0297595052710396,
1.52405718851832));
#16195=CARTESIAN_POINT('Ctrl Pts',(0.123464283518865,0.0254385629829291,
1.52387764960816));
#16196=CARTESIAN_POINT('Ctrl Pts',(0.124512110981915,0.0210533134598664,
1.52369838877875));
#16197=CARTESIAN_POINT('Ctrl Pts',(0.12532867129748,0.0166220814218575,
1.52351913980531));
#16198=CARTESIAN_POINT('Ctrl Pts',(0.126067828800149,0.012610891624201,
1.52335688207487));
#16199=CARTESIAN_POINT('Ctrl Pts',(0.12661735951473,0.00855739899605222,
1.52319445303817));
#16200=CARTESIAN_POINT('Ctrl Pts',(0.126966826155483,0.00450415768051923,
1.52303280899981));
#16201=CARTESIAN_POINT('Ctrl Pts',(0.127602972227412,-0.00287409603749457,
1.52273856283131));
#16202=CARTESIAN_POINT('Ctrl Pts',(0.12758177643555,-0.010267620141741,
1.52244625042084));
#16203=CARTESIAN_POINT('Ctrl Pts',(0.126865581413421,-0.0175939782534482,
1.52215473434257));
#16204=CARTESIAN_POINT('Ctrl Pts',(0.126426462283551,-0.0220859726121444,
1.52197599770985));
#16205=CARTESIAN_POINT('Ctrl Pts',(0.12572570473317,-0.0265528301690258,
1.52179756043894));
#16206=CARTESIAN_POINT('Ctrl Pts',(0.124776542651163,-0.0309793260681717,
1.52161916036391));
#16207=CARTESIAN_POINT('Ctrl Pts',(0.124151644840291,-0.0338935887106027,
1.52150170748789));
#16208=CARTESIAN_POINT('Ctrl Pts',(0.123418330834614,-0.0367926408403149,
1.52138417707714));
#16209=CARTESIAN_POINT('Ctrl Pts',(0.122581975874549,-0.0396644408336013,
1.52126680258073));
#16210=CARTESIAN_POINT('Ctrl Pts',(0.120074191833131,-0.0482754427851461,
1.52091485884509));
#16211=CARTESIAN_POINT('Ctrl Pts',(0.116656903439717,-0.0566007293654626,
1.52056600333313));
#16212=CARTESIAN_POINT('Ctrl Pts',(0.112443760417108,-0.0645262187619275,
1.52021830866717));
#16213=CARTESIAN_POINT('Ctrl Pts',(0.109356904590302,-0.0703330102694749,
1.51996356219884));
#16214=CARTESIAN_POINT('Ctrl Pts',(0.105841781173658,-0.0759253337267248,
1.51970943888381));
#16215=CARTESIAN_POINT('Ctrl Pts',(0.101930367117466,-0.0812537151913617,
1.51945518067311));
#16216=CARTESIAN_POINT('Ctrl Pts',(0.100130771446666,-0.0837052409256295,
1.51933819945644));
#16217=CARTESIAN_POINT('Ctrl Pts',(0.0982476276828181,-0.0860996963839449,
1.51922123442864));
#16218=CARTESIAN_POINT('Ctrl Pts',(0.0962924325256194,-0.0884227179472683,
1.51910469697823));
#16219=CARTESIAN_POINT('Ctrl Pts',(0.0906946176521128,-0.0950736369671782,
1.51877104482549));
#16220=CARTESIAN_POINT('Ctrl Pts',(0.0844921899154374,-0.101162815315101,
1.51843983772287));
#16221=CARTESIAN_POINT('Ctrl Pts',(0.0777644521522082,-0.106582693579069,
1.51810941878));
#16222=CARTESIAN_POINT('Ctrl Pts',(0.0731067700043679,-0.110334931124879,
1.5178806663426));
#16223=CARTESIAN_POINT('Ctrl Pts',(0.0681966627772886,-0.113766151308436,
1.51765229166508));
#16224=CARTESIAN_POINT('Ctrl Pts',(0.0630541948599911,-0.116833686038022,
1.5174237449583));
#16225=CARTESIAN_POINT('Ctrl Pts',(0.0607686815400033,-0.118197018118406,
1.51732216988754));
#16226=CARTESIAN_POINT('Ctrl Pts',(0.0584414404741937,-0.119485783651375,
1.51722075040181));
#16227=CARTESIAN_POINT('Ctrl Pts',(0.0560784264268894,-0.12069488199044,
1.51711960151386));
#16228=CARTESIAN_POINT('Ctrl Pts',(0.0475595529450054,-0.125053787850271,
1.51675495087613));
#16229=CARTESIAN_POINT('Ctrl Pts',(0.038563113830939,-0.128389854466075,
1.51639315730301));
#16230=CARTESIAN_POINT('Ctrl Pts',(0.0292711048986314,-0.130741856378471,
1.51603205677802));
#16231=CARTESIAN_POINT('Ctrl Pts',(0.0254547302664753,-0.13170786066222,
1.51588374709674));
#16232=CARTESIAN_POINT('Ctrl Pts',(0.0215881861914954,-0.132507324978224,
1.51573555432397));
#16233=CARTESIAN_POINT('Ctrl Pts',(0.0176832233642019,-0.13314066674995,
1.51558732853105));
#16234=CARTESIAN_POINT('Ctrl Pts',(0.0144414794405867,-0.133666441752394,
1.51546427740745));
#16235=CARTESIAN_POINT('Ctrl Pts',(0.0111713231872828,-0.134077605234841,
1.5153411329761));
#16236=CARTESIAN_POINT('Ctrl Pts',(0.00789687394913892,-0.134372952697723,
1.51521845803943));
#16237=CARTESIAN_POINT('Ctrl Pts',(-0.00208492598009478,-0.135273287095873,
1.51484449692866));
#16238=CARTESIAN_POINT('Ctrl Pts',(-0.0121386692885745,-0.135107999768821,
1.51447364169918));
#16239=CARTESIAN_POINT('Ctrl Pts',(-0.0220717676774029,-0.133899092645375,
1.51410356562093));
#16240=CARTESIAN_POINT('Ctrl Pts',(-0.0271373055616968,-0.133282591671289,
1.51391483957382));
#16241=CARTESIAN_POINT('Ctrl Pts',(-0.0321716696217597,-0.132393849601707,
1.51372631615657));
#16242=CARTESIAN_POINT('Ctrl Pts',(-0.0371491047637803,-0.131230566976147,
1.51353768678866));
#16243=CARTESIAN_POINT('Ctrl Pts',(-0.0401763453142056,-0.130523066780721,
1.51342296375255));
#16244=CARTESIAN_POINT('Ctrl Pts',(-0.0431793745847511,-0.129714439573166,
1.51330831773957));
#16245=CARTESIAN_POINT('Ctrl Pts',(-0.0461427198170546,-0.128807808452418,
1.51319405707679));
#16246=CARTESIAN_POINT('Ctrl Pts',(-0.0557912886485991,-0.125855842991896,
1.51282202756853));
#16247=CARTESIAN_POINT('Ctrl Pts',(-0.0650506639775802,-0.121862017750276,
1.51245293010828));
#16248=CARTESIAN_POINT('Ctrl Pts',(-0.0737251756215706,-0.116823260910032,
1.51208446868514));
#16249=CARTESIAN_POINT('Ctrl Pts',(-0.0774533877539874,-0.114657657224767,
1.51192610791459));
#16250=CARTESIAN_POINT('Ctrl Pts',(-0.0810733781510443,-0.112298364258586,
1.51176786463208));
#16251=CARTESIAN_POINT('Ctrl Pts',(-0.0845783705992567,-0.109758519633299,
1.51160955655689));
#16252=CARTESIAN_POINT('Ctrl Pts',(-0.0871260289206952,-0.107912394030924,
1.51149448786814));
#16253=CARTESIAN_POINT('Ctrl Pts',(-0.0896122610481647,-0.105970921032248,
1.51137940572563));
#16254=CARTESIAN_POINT('Ctrl Pts',(-0.0920243025666997,-0.10394826075131,
1.51126473391974));
#16255=CARTESIAN_POINT('Ctrl Pts',(-0.0995315444015674,-0.0976529296958118,
1.51090782920982));
#16256=CARTESIAN_POINT('Ctrl Pts',(-0.106349817996106,-0.090554906599088,
1.51055366538392));
#16257=CARTESIAN_POINT('Ctrl Pts',(-0.112409916721278,-0.0828189535999138,
1.51020021897155));
#16258=CARTESIAN_POINT('Ctrl Pts',(-0.11567060314877,-0.0786565598680515,
1.51001004419521));
#16259=CARTESIAN_POINT('Ctrl Pts',(-0.118711357121208,-0.0743087544864998,
1.50982007711492));
#16260=CARTESIAN_POINT('Ctrl Pts',(-0.121517490738653,-0.0697974244982526,
1.50963000253165));
#16261=CARTESIAN_POINT('Ctrl Pts',(-0.123184827969132,-0.0671169005197731,
1.50951706477726));
#16262=CARTESIAN_POINT('Ctrl Pts',(-0.124768226583796,-0.064379797453554,
1.50940414472167));
#16263=CARTESIAN_POINT('Ctrl Pts',(-0.12625918933752,-0.0616017405091787,
1.50929161182319));
#16264=CARTESIAN_POINT('Ctrl Pts',(-0.131254477666307,-0.0522942005345653,
1.50891458411209));
#16265=CARTESIAN_POINT('Ctrl Pts',(-0.135235816373665,-0.0424980109473837,
1.50854057440173));
#16266=CARTESIAN_POINT('Ctrl Pts',(-0.138100316247284,-0.0323932585971084,
1.50816719719795));
#16267=CARTESIAN_POINT('Ctrl Pts',(-0.139428601593765,-0.027707625827389,
1.5079940600046));
#16268=CARTESIAN_POINT('Ctrl Pts',(-0.140516076092011,-0.0229552175461711,
1.50782105881478));
#16269=CARTESIAN_POINT('Ctrl Pts',(-0.14134846970832,-0.01815262603916,
1.50764795577689));
#16270=CARTESIAN_POINT('Ctrl Pts',(-0.141840021659925,-0.0153165600461233,
1.5075457335416));
#16271=CARTESIAN_POINT('Ctrl Pts',(-0.142241997144177,-0.0124651428186592,
1.50744355431084));
#16272=CARTESIAN_POINT('Ctrl Pts',(-0.142550993842162,-0.00961078035088443,
1.50734168592779));
#16273=CARTESIAN_POINT('Ctrl Pts',(-0.142847161918882,-0.00687492249914849,
1.50724404681617));
#16274=CARTESIAN_POINT('Ctrl Pts',(-0.143058332724879,-0.00413406598225375,
1.5071466105924));
#16275=CARTESIAN_POINT('Ctrl Pts',(-0.143182669649515,-0.00139134585336764,
1.50704933585643));
#16276=CARTESIAN_POINT('Ctrl Pts',(-0.143203595382121,-0.00092974984559876,
1.50703296465278));
#16277=CARTESIAN_POINT('Ctrl Pts',(-0.143222061023464,-0.000468100854706259,
1.50701659802318));
#16278=CARTESIAN_POINT('Ctrl Pts',(-0.143238079070951,-6.41379011939899E-6,
1.50700023577028));
#16279=CARTESIAN_POINT('',(-0.00156744678985144,0.146109855568756,1.50365));
#16280=CARTESIAN_POINT('Ctrl Pts',(-0.00156962371672063,0.146072546381438,
1.50365));
#16281=CARTESIAN_POINT('Ctrl Pts',(-0.011711474284147,0.144648739717271,
1.50495065132295));
#16282=CARTESIAN_POINT('Ctrl Pts',(-0.0216501921041044,0.142222471223284,
1.50626105010813));
#16283=CARTESIAN_POINT('Ctrl Pts',(-0.0312062965385204,0.138804788898175,
1.50759029209282));
#16284=CARTESIAN_POINT('Ctrl Pts',(-0.0379863325344082,0.136379950477271,
1.50853338648503));
#16285=CARTESIAN_POINT('Ctrl Pts',(-0.0445735484268955,0.133455002060128,
1.5094859663039));
#16286=CARTESIAN_POINT('Ctrl Pts',(-0.0508923708069948,0.130021662144985,
1.51045128011208));
#16287=CARTESIAN_POINT('Ctrl Pts',(-0.053607485163773,0.128546401418451,
1.51086606268101));
#16288=CARTESIAN_POINT('Ctrl Pts',(-0.0562647183424556,0.126981576978965,
1.51128195276517));
#16289=CARTESIAN_POINT('Ctrl Pts',(-0.0588579379029418,0.125328026221608,
1.51169910067666));
#16290=CARTESIAN_POINT('Ctrl Pts',(-0.0624505046767585,0.123037247762191,
1.51227700458785));
#16291=CARTESIAN_POINT('Ctrl Pts',(-0.0659209207101175,0.120575889029892,
1.51285741907924));
#16292=CARTESIAN_POINT('Ctrl Pts',(-0.0692542752175272,0.117943487410649,
1.51344114883776));
#16293=CARTESIAN_POINT('Ctrl Pts',(-0.0735613784355843,0.114542101371374,
1.51419539934302));
#16294=CARTESIAN_POINT('Ctrl Pts',(-0.0776398170223455,0.110855132244726,
1.51495518495604));
#16295=CARTESIAN_POINT('Ctrl Pts',(-0.0814741368103916,0.106911749311875,
1.51572224163114));
#16296=CARTESIAN_POINT('Ctrl Pts',(-0.0845038784997064,0.103795829845314,
1.51632834224744));
#16297=CARTESIAN_POINT('Ctrl Pts',(-0.087381117690253,0.10051973853988,
1.51693898261853));
#16298=CARTESIAN_POINT('Ctrl Pts',(-0.0900959757046659,0.0970973798321736,
1.51755501917095));
#16299=CARTESIAN_POINT('Ctrl Pts',(-0.0920052356275281,0.0946905606587243,
1.51798825505079));
#16300=CARTESIAN_POINT('Ctrl Pts',(-0.093830595110286,0.092215607777745,
1.51842338946406));
#16301=CARTESIAN_POINT('Ctrl Pts',(-0.0955653742165971,0.0896840982544811,
1.51885969689116));
#16302=CARTESIAN_POINT('Ctrl Pts',(-0.0997851775729162,0.0835262696618028,
1.51992100293214));
#16303=CARTESIAN_POINT('Ctrl Pts',(-0.103479134251024,0.0770231540939269,
1.52099120961793));
#16304=CARTESIAN_POINT('Ctrl Pts',(-0.106606394578922,0.0702509006766953,
1.52207541818308));
#16305=CARTESIAN_POINT('Ctrl Pts',(-0.108879606303698,0.0653281362576702,
1.52286353153598));
#16306=CARTESIAN_POINT('Ctrl Pts',(-0.110852991156964,0.0602629640702717,
1.52365904329275));
#16307=CARTESIAN_POINT('Ctrl Pts',(-0.112503888351057,0.0550849881514033,
1.524463912762));
#16308=CARTESIAN_POINT('Ctrl Pts',(-0.113450017754745,0.0521174894567802,
1.52492518356294));
#16309=CARTESIAN_POINT('Ctrl Pts',(-0.114289979676541,0.0491121240008169,
1.52538965304266));
#16310=CARTESIAN_POINT('Ctrl Pts',(-0.115015874151616,0.0460903162170444,
1.52585530945224));
#16311=CARTESIAN_POINT('Ctrl Pts',(-0.117053612444637,0.0376074669234184,
1.52716250482259));
#16312=CARTESIAN_POINT('Ctrl Pts',(-0.118206139871793,0.0289652499882669,
1.52848357355921));
#16313=CARTESIAN_POINT('Ctrl Pts',(-0.11838625730212,0.0202925750432425,
1.52982832573377));
#16314=CARTESIAN_POINT('Ctrl Pts',(-0.118492077855379,0.015197303257165,
1.53061837930521));
#16315=CARTESIAN_POINT('Ctrl Pts',(-0.118261361656021,0.0100916471271278,
1.53141660760476));
#16316=CARTESIAN_POINT('Ctrl Pts',(-0.11766859746431,0.00500517689818842,
1.532225));
#16317=CARTESIAN_POINT('',(-0.115079981391543,0.0902137050004572,1.50365));
#16318=CARTESIAN_POINT('Origin',(0.,0.,1.50365));
#16319=CARTESIAN_POINT('Ctrl Pts',(-0.143238079070951,-6.41379011939899E-6,
1.50700023577028));
#16320=CARTESIAN_POINT('Ctrl Pts',(-0.143514357617001,0.00795674345750163,
1.50671802038504));
#16321=CARTESIAN_POINT('Ctrl Pts',(-0.14306421847979,0.0159310909218757,
1.50643710681857));
#16322=CARTESIAN_POINT('Ctrl Pts',(-0.141940608246003,0.023841490005315,
1.50615648267927));
#16323=CARTESIAN_POINT('Ctrl Pts',(-0.141317731836386,0.0282266413964,1.50600091791928));
#16324=CARTESIAN_POINT('Ctrl Pts',(-0.14048752132733,0.0325921818867556,
1.50584544210227));
#16325=CARTESIAN_POINT('Ctrl Pts',(-0.139456452513291,0.0369250818702156,
1.5056898827608));
#16326=CARTESIAN_POINT('Ctrl Pts',(-0.138790989895207,0.0397215809279161,
1.50558948313156));
#16327=CARTESIAN_POINT('Ctrl Pts',(-0.138042009924554,0.0425029011667524,
1.50548910366784));
#16328=CARTESIAN_POINT('Ctrl Pts',(-0.137214434473447,0.0452564915355094,
1.50538902890071));
#16329=CARTESIAN_POINT('Ctrl Pts',(-0.134176751889031,0.0553637675507716,
1.50502169637912));
#16330=CARTESIAN_POINT('Ctrl Pts',(-0.130076454936343,0.0651325632434767,
1.50465723703036));
#16331=CARTESIAN_POINT('Ctrl Pts',(-0.125018127980614,0.0743940890034878,
1.50429344851366));
#16332=CARTESIAN_POINT('Ctrl Pts',(-0.122034683484208,0.0798566160996726,
1.50407888293545));
#16333=CARTESIAN_POINT('Ctrl Pts',(-0.118716925567465,0.0851425936725427,
1.50386455072235));
#16334=CARTESIAN_POINT('Ctrl Pts',(-0.115078604842436,0.0902138214954005,
1.50365));
#16335=CARTESIAN_POINT('',(-0.05,-6.12323399573677E-18,1.6));
#16336=CARTESIAN_POINT('',(-0.1,-1.22464679914735E-17,1.55));
#16337=CARTESIAN_POINT('Origin',(0.,0.,1.6));
#16338=CARTESIAN_POINT('Ctrl Pts',(0.0850780204044575,-0.11908002747757,
-0.0164977839420936));
#16339=CARTESIAN_POINT('Ctrl Pts',(0.124677800165771,-0.0907875342533835,
-0.0138514540629917));
#16340=CARTESIAN_POINT('Ctrl Pts',(0.172751483861701,0.00791416360185712,
-0.00855879430478784));
#16341=CARTESIAN_POINT('Ctrl Pts',(0.0868617128612901,0.149726167188418,
-0.000619804667482127));
#16342=CARTESIAN_POINT('Ctrl Pts',(-0.078614020905812,0.154028602276276,
0.00731918496982359));
#16343=CARTESIAN_POINT('Ctrl Pts',(-0.172087192378165,0.0175525219725009,
0.0152581746071293));
#16344=CARTESIAN_POINT('Ctrl Pts',(-0.108045720411827,-0.135108484733225,
0.0231971642444351));
#16345=CARTESIAN_POINT('Ctrl Pts',(0.0549144151285058,-0.164025561655164,
0.0311361538817407));
#16346=CARTESIAN_POINT('Ctrl Pts',(0.167598788591005,-0.0428207868793744,
0.0390751435190465));
#16347=CARTESIAN_POINT('Ctrl Pts',(0.126860790413016,0.117600499296196,
0.0470141331563521));
#16348=CARTESIAN_POINT('Ctrl Pts',(-0.0300110592737492,0.170357625684536,
0.054953122793658));
#16349=CARTESIAN_POINT('Ctrl Pts',(-0.159409054995301,0.0671687418111174,
0.0628921124309635));
#16350=CARTESIAN_POINT('Ctrl Pts',(-0.142879399887002,-0.0975110083167992,
0.0708311020682695));
#16351=CARTESIAN_POINT('Ctrl Pts',(0.00444677171871267,-0.172924803493063,
0.078770091705575));
#16352=CARTESIAN_POINT('Ctrl Pts',(0.147702113712341,-0.0900384822365835,
0.0867090813428809));
#16353=CARTESIAN_POINT('Ctrl Pts',(0.155746353789385,0.0752722621313087,
0.0946480709801864));
#16354=CARTESIAN_POINT('Ctrl Pts',(0.021215449100004,0.17167621786987,0.102587060617492));
#16355=CARTESIAN_POINT('Ctrl Pts',(-0.132736728465598,0.110922462699857,
0.110526050254798));
#16356=CARTESIAN_POINT('Ctrl Pts',(-0.165177537004225,-0.0513732581591355,
0.118465039892104));
#16357=CARTESIAN_POINT('Ctrl Pts',(-0.0464096261145344,-0.166640254043574,
0.126404029529409));
#16358=CARTESIAN_POINT('Ctrl Pts',(0.114843114370719,-0.129359532685675,
0.134343019166715));
#16359=CARTESIAN_POINT('Ctrl Pts',(0.170964855654229,0.0263409830179588,
0.142282008804021));
#16360=CARTESIAN_POINT('Ctrl Pts',(0.0705799878925336,0.157928129946847,
0.150220998441327));
#16361=CARTESIAN_POINT('Ctrl Pts',(-0.0944160212638482,0.144942899583874,
0.158159988078632));
#16362=CARTESIAN_POINT('Ctrl Pts',(-0.172980633894512,-0.000727622896455919,
0.166098977715938));
#16363=CARTESIAN_POINT('Ctrl Pts',(-0.0931933312323777,-0.145732055885043,
0.174037967353244));
#16364=CARTESIAN_POINT('Ctrl Pts',(0.0719060791645076,-0.157328779695546,
0.181976956990549));
#16365=CARTESIAN_POINT('Ctrl Pts',(0.171180402159323,-0.0249017879745179,
0.189915946627855));
#16366=CARTESIAN_POINT('Ctrl Pts',(0.113750798721884,0.13032108391891,0.197854936265161));
#16367=CARTESIAN_POINT('Ctrl Pts',(-0.0478098650864174,0.16624393501773,
0.205793925902467));
#16368=CARTESIAN_POINT('Ctrl Pts',(-0.16560387403618,0.0499818570245514,
0.213732915539772));
#16369=CARTESIAN_POINT('Ctrl Pts',(-0.131798885878402,-0.112035185581475,
0.221671905177078));
#16370=CARTESIAN_POINT('Ctrl Pts',(0.0226589495323734,-0.171491694067101,
0.229610894814384));
#16371=CARTESIAN_POINT('Ctrl Pts',(0.156374069566079,-0.073959309724122,
0.237549884451689));
#16372=CARTESIAN_POINT('Ctrl Pts',(0.146939445926624,0.0912777539068999,
0.245488874088995));
#16373=CARTESIAN_POINT('Ctrl Pts',(0.00299182995941577,0.172956289510158,
0.253427863726301));
#16374=CARTESIAN_POINT('Ctrl Pts',(-0.143694601292225,0.0963051955349955,
0.261366853363607));
#16375=CARTESIAN_POINT('Ctrl Pts',(-0.15883847309497,-0.0685067047260848,
0.269305843000912));
#16376=CARTESIAN_POINT('Ctrl Pts',(-0.0285766086907934,-0.170605411881679,
0.277244832638218));
#16377=CARTESIAN_POINT('Ctrl Pts',(0.12784518248692,-0.116526556812001,
0.285183822275524));
#16378=CARTESIAN_POINT('Ctrl Pts',(0.167233470900423,0.0442243749325307,
0.293122811912829));
#16379=CARTESIAN_POINT('Ctrl Pts',(0.0535309779628647,0.164490922320707,
0.301061801550136));
#16380=CARTESIAN_POINT('Ctrl Pts',(-0.109175456582181,0.134177303623408,
0.309000791187441));
#16381=CARTESIAN_POINT('Ctrl Pts',(-0.171939242908932,-0.0189664407699395,
0.316939780824747));
#16382=CARTESIAN_POINT('Ctrl Pts',(-0.0773044361184472,-0.154747708493488,
0.324878770462053));
#16383=CARTESIAN_POINT('Ctrl Pts',(0.0880972839194656,-0.148868054644337,
0.332817760099358));
#16384=CARTESIAN_POINT('Ctrl Pts',(0.172851978230285,-0.00670989936239309,
0.340756749736664));
#16385=CARTESIAN_POINT('Ctrl Pts',(0.0993725327910066,0.141590708926387,
0.34869573937397));
#16386=CARTESIAN_POINT('Ctrl Pts',(-0.0650756559739905,0.160274727038081,
0.356634729011275));
#16387=CARTESIAN_POINT('Ctrl Pts',(-0.169951541620772,0.0322382168908211,
0.364573718648582));
#16388=CARTESIAN_POINT('Ctrl Pts',(-0.119248438453561,-0.125310171390688,
0.372512708285886));
#16389=CARTESIAN_POINT('Ctrl Pts',(0.0406184374886585,-0.168145685830938,
0.380451697923193));
#16390=CARTESIAN_POINT('Ctrl Pts',(0.163301917673335,-0.0570553486694088,
0.388390687560498));
#16391=CARTESIAN_POINT('Ctrl Pts',(0.136493684039406,0.106265249940549,
0.396329677197804));
#16392=CARTESIAN_POINT('Ctrl Pts',(-0.0152651628095069,0.172307295063139,
0.404268666835109));
#16393=CARTESIAN_POINT('Ctrl Pts',(-0.153049799296248,0.0806138205455782,
0.412207656472416));
#16394=CARTESIAN_POINT('Ctrl Pts',(-0.150727833715048,-0.0848760818555219,
0.420146646109721));
#16395=CARTESIAN_POINT('Ctrl Pts',(-0.0104248664208018,-0.172667748255674,
0.428085635747027));
#16396=CARTESIAN_POINT('Ctrl Pts',(0.139421351618932,-0.10239392482138,
0.436024625384332));
#16397=CARTESIAN_POINT('Ctrl Pts',(0.16163687742079,0.0616145192729195,
0.443963615021638));
#16398=CARTESIAN_POINT('Ctrl Pts',(0.0358849196425865,0.169219093691645,
0.451902604658944));
#16399=CARTESIAN_POINT('Ctrl Pts',(-0.122717222714247,0.121915185177559,
0.45984159429625));
#16400=CARTESIAN_POINT('Ctrl Pts',(-0.168980158036723,-0.0369937199732681,
0.467780583933555));
#16401=CARTESIAN_POINT('Ctrl Pts',(-0.0605533396431397,-0.162037409833775,
0.475719573570861));
#16402=CARTESIAN_POINT('Ctrl Pts',(0.103305911202344,-0.138746956140414,
0.483658563208167));
#16403=CARTESIAN_POINT('Ctrl Pts',(0.172595680358559,0.0115568269495825,
0.491597552845473));
#16404=CARTESIAN_POINT('Ctrl Pts',(0.0838859329010004,0.151281127008313,
0.499536542482778));
#16405=CARTESIAN_POINT('Ctrl Pts',(-0.0816156370489812,0.152517923263679,
0.507475532120084));
#16406=CARTESIAN_POINT('Ctrl Pts',(-0.172403684765527,0.0141350135070757,
0.51541452175739));
#16407=CARTESIAN_POINT('Ctrl Pts',(-0.105367974675403,-0.137187532379513,
0.523353511394695));
#16408=CARTESIAN_POINT('Ctrl Pts',(0.0581248948911363,-0.162924294448283,
0.531292501032001));
#16409=CARTESIAN_POINT('Ctrl Pts',(0.168408406744046,-0.039515030880773,
0.539231490669306));
#16410=CARTESIAN_POINT('Ctrl Pts',(0.124525564004667,0.120067535316156,
0.547170480306613));
#16411=CARTESIAN_POINT('Ctrl Pts',(-0.0333518982867267,0.169736501696743,
0.555109469943918));
#16412=CARTESIAN_POINT('Ctrl Pts',(-0.160697983451488,0.0640233335761385,
0.563048459581225));
#16413=CARTESIAN_POINT('Ctrl Pts',(-0.14093607811848,-0.100298808627811,
0.570987449218529));
#16414=CARTESIAN_POINT('Ctrl Pts',(0.00784314775175556,-0.172804265459278,
0.578926438855836));
#16415=CARTESIAN_POINT('Ctrl Pts',(0.149442509381278,-0.0871192603125336,
0.586865428493141));
#16416=CARTESIAN_POINT('Ctrl Pts',(0.154237495636292,0.0783174569774929,
0.594804418130446));
#16417=CARTESIAN_POINT('Ctrl Pts',(0.0178386252221998,0.172059909850489,
0.602743407767753));
#16418=CARTESIAN_POINT('Ctrl Pts',(-0.134890284021987,0.108293307291099,
0.610682397405058));
#16419=CARTESIAN_POINT('Ctrl Pts',(-0.164136382878957,-0.0546083962682395,
0.618621387042364));
#16420=CARTESIAN_POINT('Ctrl Pts',(-0.0431268722112106,-0.167519855601819,
0.62656037667967));
#16421=CARTESIAN_POINT('Ctrl Pts',(0.117362334288317,-0.127078368017432,
0.634499366316975));
#16422=CARTESIAN_POINT('Ctrl Pts',(0.170414367112955,0.0296946562375699,
0.642438355954282));
#16423=CARTESIAN_POINT('Ctrl Pts',(0.0674637261050104,0.159284257814778,
0.650377345591586));
#16424=CARTESIAN_POINT('Ctrl Pts',(-0.0972453325609638,0.143060037825677,
0.658316335228894));
#16425=CARTESIAN_POINT('Ctrl Pts',(-0.172932953925271,-0.00412584224812367,
0.666255324866198));
#16426=CARTESIAN_POINT('Ctrl Pts',(-0.0903123078403481,-0.147534796506203,
0.674194314503505));
#16427=CARTESIAN_POINT('Ctrl Pts',(0.0749830665657334,-0.155885755782802,
0.68213330414081));
#16428=CARTESIAN_POINT('Ctrl Pts',(0.17163658245605,-0.021533989188811,
0.690072293778116));
#16429=CARTESIAN_POINT('Ctrl Pts',(0.11116857013107,0.132530668686874,0.698011283415421));
#16430=CARTESIAN_POINT('Ctrl Pts',(-0.0510666492692211,0.165272582299639,
0.705950273052727));
#16431=CARTESIAN_POINT('Ctrl Pts',(-0.166553851089581,0.0467187736868841,
0.713889262690032));
#16432=CARTESIAN_POINT('Ctrl Pts',(-0.129572416918314,-0.114602870389546,
0.721828252327339));
#16433=CARTESIAN_POINT('Ctrl Pts',(0.0260236847639906,-0.171013440871999,
0.729767241964644));
#16434=CARTESIAN_POINT('Ctrl Pts',(0.157796886564457,-0.0708729265526718,
0.73770623160195));
#16435=CARTESIAN_POINT('Ctrl Pts',(0.145117853242075,0.0941468947867542,
0.745645221239255));
#16436=CARTESIAN_POINT('Ctrl Pts',(-0.000406629147419015,0.172981686256994,
0.753584210876562));
#16437=CARTESIAN_POINT('Ctrl Pts',(-0.145558870420566,0.0934635991681543,
0.761523200513868));
#16438=CARTESIAN_POINT('Ctrl Pts',(-0.157461941624574,-0.0716140074803496,
0.769462190151172));
#16439=CARTESIAN_POINT('Ctrl Pts',(-0.0252193968429213,-0.17113389830906,
0.777401179788479));
#16440=CARTESIAN_POINT('Ctrl Pts',(0.130109777350283,-0.113992433807847,
0.785340169425784));
#16441=CARTESIAN_POINT('Ctrl Pts',(0.166332367384696,0.0475012914327479,
0.793279159063091));
#16442=CARTESIAN_POINT('Ctrl Pts',(0.0502890745800368,0.165510839842773,
0.801218148700395));
#16443=CARTESIAN_POINT('Ctrl Pts',(-0.111790419467279,0.132006557575396,
0.809157138337702));
#16444=CARTESIAN_POINT('Ctrl Pts',(-0.171533445990104,-0.0223406811520247,
0.817096127975007));
#16445=CARTESIAN_POINT('Ctrl Pts',(-0.0742493586638003,-0.156236557391639,
0.825035117612313));
#16446=CARTESIAN_POINT('Ctrl Pts',(0.0910049278783345,-0.147108572929777,
0.832974107249618));
#16447=CARTESIAN_POINT('Ctrl Pts',(0.172950439922886,-0.00331277195964383,
0.840913096886925));
#16448=CARTESIAN_POINT('Ctrl Pts',(0.0965716772857839,0.143515644700454,
0.848852086524229));
#16449=CARTESIAN_POINT('Ctrl Pts',(-0.0682118374171683,0.158965324406771,
0.856791076161536));
#16450=CARTESIAN_POINT('Ctrl Pts',(-0.170552089827228,0.0288931442238776,
0.864730065798841));
#16451=CARTESIAN_POINT('Ctrl Pts',(-0.116763592698541,-0.127628729319482,
0.872669055436147));
#16452=CARTESIAN_POINT('Ctrl Pts',(0.0439139712140358,-0.167315248138923,
0.880608045073453));
#16453=CARTESIAN_POINT('Ctrl Pts',(0.164391304101163,-0.0538361241500125,
0.888547034710759));
#16454=CARTESIAN_POINT('Ctrl Pts',(0.134379664555536,0.108926281867684,
0.896486024348063));
#16455=CARTESIAN_POINT('Ctrl Pts',(-0.018647348250808,0.17197414204115,
0.904425013985371));
#16456=CARTESIAN_POINT('Ctrl Pts',(-0.154603991719776,0.0775914613336281,
0.912364003622676));
#16457=CARTESIAN_POINT('Ctrl Pts',(-0.149031276472826,-0.0878208845346985,
0.920302993259982));
#16458=CARTESIAN_POINT('Ctrl Pts',(-0.00703064139541984,-0.172839229369798,
0.928241982897287));
#16459=CARTESIAN_POINT('Ctrl Pts',(0.141406064038169,-0.099635105162837,
0.936180972534593));
#16460=CARTESIAN_POINT('Ctrl Pts',(0.160395209035295,0.064778129380991,
0.944119962171899));
#16461=CARTESIAN_POINT('Ctrl Pts',(0.03255353276219,0.169891426011666,0.952058951809204));
#16462=CARTESIAN_POINT('Ctrl Pts',(-0.125088671715395,0.119480765548496,
0.959997941446511));
#16463=CARTESIAN_POINT('Ctrl Pts',(-0.168220770124088,-0.040306347222682,
0.967936931083815));
#16464=CARTESIAN_POINT('Ctrl Pts',(-0.0573582824064844,-0.163195761485875,
0.975875920721122));
#16465=CARTESIAN_POINT('Ctrl Pts',(0.106011781834435,-0.136690640644722,
0.983814910358427));
#16466=CARTESIAN_POINT('Ctrl Pts',(0.17233532526783,0.014945393685262,0.991753899995733));
#16467=CARTESIAN_POINT('Ctrl Pts',(0.0808976893297158,0.152899944371113,
0.999692889633039));
#16468=CARTESIAN_POINT('Ctrl Pts',(-0.0845962369090198,0.150885074902754,
1.00763187927034));
#16469=CARTESIAN_POINT('Ctrl Pts',(-0.172648106016301,0.0107452601904448,
1.01557086890765));
#16470=CARTESIAN_POINT('Ctrl Pts',(-0.102652466413112,-0.13923110380544,
1.02350985854496));
#16471=CARTESIAN_POINT('Ctrl Pts',(0.0613144709582997,-0.161750934398167,
1.03144884818226));
#16472=CARTESIAN_POINT('Ctrl Pts',(0.169152212322519,-0.0361988700648799,
1.03938783781957));
#16473=CARTESIAN_POINT('Ctrl Pts',(0.122142696063681,0.12249077894222,1.04732682745687));
#16474=CARTESIAN_POINT('Ctrl Pts',(-0.0366800874558037,0.169048514669047,
1.05526581709418));
#16475=CARTESIAN_POINT('Ctrl Pts',(-0.161924764760067,0.0608539208677085,
1.06320480673148));
#16476=CARTESIAN_POINT('Ctrl Pts',(-0.138938417355371,-0.103048266896446,
1.07114379636879));
#16477=CARTESIAN_POINT('Ctrl Pts',(0.011236529066559,-0.172616828675865,
1.0790827860061));
#16478=CARTESIAN_POINT('Ctrl Pts',(0.151125203217684,-0.0841665140064042,
1.0870217756434));
#16479=CARTESIAN_POINT('Ctrl Pts',(0.152669111109608,0.0813324759279986,
1.09496076528071));
#16480=CARTESIAN_POINT('Ctrl Pts',(0.0144549108781955,0.172377158228925,
1.10289975491801));
#16481=CARTESIAN_POINT('Ctrl Pts',(-0.136991769602464,0.10562236594946,
1.11083874455532));
#16482=CARTESIAN_POINT('Ctrl Pts',(-0.163031873671196,-0.0578224635832477,
1.11877773419263));
#16483=CARTESIAN_POINT('Ctrl Pts',(-0.0398274706979539,-0.168334790537727,
1.12671672382993));
#16484=CARTESIAN_POINT('Ctrl Pts',(0.119836252144435,-0.124748153491552,
1.13465571346724));
#16485=CARTESIAN_POINT('Ctrl Pts',(0.169798099063322,0.0330368685268242,
1.14259470310454));
#16486=CARTESIAN_POINT('Ctrl Pts',(0.0643214233134591,0.160578901573361,
1.15053369274185));
#16487=CARTESIAN_POINT('Ctrl Pts',(-0.100037107244844,0.141121955420339,
1.15847268237915));
#16488=CARTESIAN_POINT('Ctrl Pts',(-0.172818522111203,-0.00752246920075927,
1.16641167201646));
#16489=CARTESIAN_POINT('Ctrl Pts',(-0.0873964240115842,-0.149280588817046,
1.17435066165376));
#16490=CARTESIAN_POINT('Ctrl Pts',(0.0780311106025284,-0.154382560238235,
1.18228965129107));
#16491=CARTESIAN_POINT('Ctrl Pts',(0.172026511281289,-0.01815787828917,
1.19022864092837));
#16492=CARTESIAN_POINT('Ctrl Pts',(0.10854343062882,0.134689096792963,1.19816763056568));
#16493=CARTESIAN_POINT('Ctrl Pts',(-0.0543037217972188,0.164237434607784,
1.20610662020299));
#16494=CARTESIAN_POINT('Ctrl Pts',(-0.167439538594998,0.0434376569656869,
1.21404560984029));
#16495=CARTESIAN_POINT('Ctrl Pts',(-0.127295933190098,-0.117126318651471,
1.2219845994776));
#16496=CARTESIAN_POINT('Ctrl Pts',(0.0293783748903316,-0.170469176734012,
1.2299235891149));
#16497=CARTESIAN_POINT('Ctrl Pts',(0.159158794190081,-0.0677591865323411,
1.23786257875221));
#16498=CARTESIAN_POINT('Ctrl Pts',(0.143240245273553,0.0969796950995427,
1.24580156838952));
#16499=CARTESIAN_POINT('Ctrl Pts',(-0.00380493129617075,0.172940312320012,
1.25374055802682));
#16500=CARTESIAN_POINT('Ctrl Pts',(-0.147366954032488,0.0905859259858403,
1.26167954766413));
#16501=CARTESIAN_POINT('Ctrl Pts',(-0.156024630070406,-0.074693667330688,
1.26961853730143));
#16502=CARTESIAN_POINT('Ctrl Pts',(-0.0218524503424686,-0.171596327294885,
1.27755752693874));
#16503=CARTESIAN_POINT('Ctrl Pts',(0.132324150022753,-0.111414309889572,
1.28549651657604));
#16504=CARTESIAN_POINT('Ctrl Pts',(0.165367059817933,0.0507598725070622,
1.29343550621335));
#16505=CARTESIAN_POINT('Ctrl Pts',(0.0470277596764783,0.166466870408131,
1.30137449585065));
#16506=CARTESIAN_POINT('Ctrl Pts',(-0.114362231391601,0.129784857201791,
1.30931348548797));
#16507=CARTESIAN_POINT('Ctrl Pts',(-0.171061437441431,-0.0257062980954763,
1.31725247512526));
#16508=CARTESIAN_POINT('Ctrl Pts',(-0.071165620995849,-0.157665099140374,
1.32519146476257));
#16509=CARTESIAN_POINT('Ctrl Pts',(0.0938774439379855,-0.145292307632914,
1.33313045439988));
#16510=CARTESIAN_POINT('Ctrl Pts',(0.172982143233999,8.56343898915854E-5,
1.34106944403719));
#16511=CARTESIAN_POINT('Ctrl Pts',(0.0937335447930804,0.145385183220099,
1.34900843367449));
#16512=CARTESIAN_POINT('Ctrl Pts',(-0.0713216883190155,0.157594562185848,
1.3569474233118));
#16513=CARTESIAN_POINT('Ctrl Pts',(-0.171086806821499,0.0255369173285507,
1.3648864129491));
#16514=CARTESIAN_POINT('Ctrl Pts',(-0.114233673229396,-0.129898019862958,
1.37282540258641));
#16515=CARTESIAN_POINT('Ctrl Pts',(0.0471925482590101,-0.166420232464351,
1.38076439222371));
#16516=CARTESIAN_POINT('Ctrl Pts',(0.165417247017141,-0.0505961085897048,
1.38870338186102));
#16517=CARTESIAN_POINT('Ctrl Pts',(0.132213753266125,0.111545248710567,
1.39664237149832));
#16518=CARTESIAN_POINT('Ctrl Pts',(-0.0220222951247444,0.17157464463752,
1.40458136113563));
#16519=CARTESIAN_POINT('Ctrl Pts',(-0.156098584526576,0.0745390809398717,
1.41252035077293));
#16520=CARTESIAN_POINT('Ctrl Pts',(-0.147277046608992,-0.0907316537045687,
1.42045934041024));
#16521=CARTESIAN_POINT('Ctrl Pts',(-0.00363398118293899,-0.172944250658386,
1.42839833004755));
#16522=CARTESIAN_POINT('Ctrl Pts',(0.143336722904634,-0.0968373407211472,
1.43633731968485));
#16523=CARTESIAN_POINT('Ctrl Pts',(0.159090624036536,0.0679158129692223,
1.44427630932216));
#16524=CARTESIAN_POINT('Ctrl Pts',(0.0292114869387437,0.170499931406899,
1.45221529895946));
#16525=CARTESIAN_POINT('Ctrl Pts',(-0.127415456569397,0.116996902323752,
1.46015428859677));
#16526=CARTESIAN_POINT('Ctrl Pts',(-0.167389576437263,-0.0435971050111283,
1.46809327823408));
#16527=CARTESIAN_POINT('Ctrl Pts',(-0.0541541359620402,-0.164303103757731,
1.47603226787138));
#16528=CARTESIAN_POINT('Ctrl Pts',(0.108701533888403,-0.13455879509903,
1.48397125750869));
#16529=CARTESIAN_POINT('Ctrl Pts',(0.171961157005542,0.0182848320604298,
1.49191024714599));
#16530=CARTESIAN_POINT('Ctrl Pts',(0.0779697431325927,0.154543202561513,
1.4998492367833));
#16531=CARTESIAN_POINT('Ctrl Pts',(-0.0877325682749983,0.149025855561406,
1.5077882264206));
#16532=CARTESIAN_POINT('Ctrl Pts',(-0.144149484752264,0.0548439265155397,
1.51308088617881));
#16533=CARTESIAN_POINT('Ctrl Pts',(-0.146217781693078,0.00621955116994065,
1.51572721605791));
#16534=CARTESIAN_POINT('Ctrl Pts',(0.0795408277542855,-0.111329858282327,
-0.0109985226280624));
#16535=CARTESIAN_POINT('Ctrl Pts',(0.116563307192903,-0.0848787452970238,
-0.00835219274896048));
#16536=CARTESIAN_POINT('Ctrl Pts',(0.16150817751539,0.00739908052493189,
-0.00305953299075667));
#16537=CARTESIAN_POINT('Ctrl Pts',(0.0812084309002137,0.139981433724326,
0.00487945664654907));
#16538=CARTESIAN_POINT('Ctrl Pts',(-0.0734975292821143,0.144003850402812,
0.0128184462838548));
#16539=CARTESIAN_POINT('Ctrl Pts',(-0.160887120581772,0.0164101388376342,
0.0207574359211605));
#16540=CARTESIAN_POINT('Ctrl Pts',(-0.101013704785435,-0.126315124179183,
0.0286964255584662));
#16541=CARTESIAN_POINT('Ctrl Pts',(0.0513403816191153,-0.153350170642076,
0.0366354151957719));
#16542=CARTESIAN_POINT('Ctrl Pts',(0.156690838735662,-0.0400338514845966,
0.0445744048330777));
#16543=CARTESIAN_POINT('Ctrl Pts',(0.118604220350264,0.109946623274354,
0.0525133944703833));
#16544=CARTESIAN_POINT('Ctrl Pts',(-0.0280578283917351,0.15927012049393,
0.0604523841076892));
#16545=CARTESIAN_POINT('Ctrl Pts',(-0.14903412333264,0.0627971513379326,
0.0683913737449947));
#16546=CARTESIAN_POINT('Ctrl Pts',(-0.133580279395553,-0.0911646307683348,
0.0763303633823007));
#16547=CARTESIAN_POINT('Ctrl Pts',(0.0041573593468571,-0.161670216863261,
0.0842693530196062));
#16548=CARTESIAN_POINT('Ctrl Pts',(0.138089113144455,-0.0841784443595545,
0.0922083426569122));
#16549=CARTESIAN_POINT('Ctrl Pts',(0.14560980428584,0.0703732645446943,
0.100147332294218));
#16550=CARTESIAN_POINT('Ctrl Pts',(0.0198346691022095,0.160502893816501,
0.108086321931524));
#16551=CARTESIAN_POINT('Ctrl Pts',(-0.124097730593135,0.103703218031488,
0.116025311568829));
#16552=CARTESIAN_POINT('Ctrl Pts',(-0.154427171169137,-0.0480296962598115,
0.123964301206135));
#16553=CARTESIAN_POINT('Ctrl Pts',(-0.0433891157712434,-0.155794689166463,
0.13190329084344));
#16554=CARTESIAN_POINT('Ctrl Pts',(0.107368699171666,-0.12094033522185,
0.139842280480747));
#16555=CARTESIAN_POINT('Ctrl Pts',(0.15983782968835,0.0246266142906177,
0.147781270118052));
#16556=CARTESIAN_POINT('Ctrl Pts',(0.0659863808909888,0.147649582370873,
0.155720259755358));
#16557=CARTESIAN_POINT('Ctrl Pts',(-0.0882710769349216,0.135509478890084,
0.163659249392663));
#16558=CARTESIAN_POINT('Ctrl Pts',(-0.161722413615419,-0.00068026650363694,
0.171598239029969));
#16559=CARTESIAN_POINT('Ctrl Pts',(-0.0871279640988751,-0.136247273976568,
0.179537228667275));
#16560=CARTESIAN_POINT('Ctrl Pts',(0.0672261652318651,-0.147089240053593,
0.187476218304581));
#16561=CARTESIAN_POINT('Ctrl Pts',(0.160039347628626,-0.023281087390596,
0.195415207941886));
#16562=CARTESIAN_POINT('Ctrl Pts',(0.106347475470598,0.121839305139765,
0.203354197579192));
#16563=CARTESIAN_POINT('Ctrl Pts',(-0.0446982220051161,0.15542416405057,
0.211293187216498));
#16564=CARTESIAN_POINT('Ctrl Pts',(-0.154825760608133,0.0467288526640558,
0.219232176853804));
#16565=CARTESIAN_POINT('Ctrl Pts',(-0.12322092627477,-0.104743520787053,
0.227171166491109));
#16566=CARTESIAN_POINT('Ctrl Pts',(0.0211842211805034,-0.160330379506191,
0.235110156128415));
#16567=CARTESIAN_POINT('Ctrl Pts',(0.146196665995071,-0.0691457639426259,
0.24304914576572));
#16568=CARTESIAN_POINT('Ctrl Pts',(0.137376082602736,0.0853370596399817,
0.250988135403027));
#16569=CARTESIAN_POINT('Ctrl Pts',(0.00279711058556459,0.161699653653757,
0.258927125040332));
#16570=CARTESIAN_POINT('Ctrl Pts',(-0.134342424474264,0.0900372967480426,
0.266866114677638));
#16571=CARTESIAN_POINT('Ctrl Pts',(-0.148500677015507,-0.0640480346713102,
0.274805104314944));
#16572=CARTESIAN_POINT('Ctrl Pts',(-0.0267167371651392,-0.159501779847699,
0.282744093952249));
#16573=CARTESIAN_POINT('Ctrl Pts',(0.119524544542348,-0.108942576944327,
0.290683083589556));
#16574=CARTESIAN_POINT('Ctrl Pts',(0.156349297273321,0.0413460888291301,
0.29862207322686));
#16575=CARTESIAN_POINT('Ctrl Pts',(0.0500469836677093,0.153785243912065,
0.306561062864167));
#16576=CARTESIAN_POINT('Ctrl Pts',(-0.102069913541897,0.125444547784578,
0.314500052501472));
#16577=CARTESIAN_POINT('Ctrl Pts',(-0.160748800211922,-0.0177320345633525,
0.322439042138778));
#16578=CARTESIAN_POINT('Ctrl Pts',(-0.0722731771226978,-0.144676154524232,
0.330378031776084));
#16579=CARTESIAN_POINT('Ctrl Pts',(0.082363586418043,-0.139179170322594,
0.338317021413389));
#16580=CARTESIAN_POINT('Ctrl Pts',(0.16160213133829,-0.00627319426210969,
0.346256011050695));
#16581=CARTESIAN_POINT('Ctrl Pts',(0.0929050003357002,0.132375461215256,
0.354195000688001));
#16582=CARTESIAN_POINT('Ctrl Pts',(-0.0608402912787218,0.149843454232904,
0.362133990325306));
#16583=CARTESIAN_POINT('Ctrl Pts',(-0.158890465884947,0.0301400343429239,
0.370072979962613));
#16584=CARTESIAN_POINT('Ctrl Pts',(-0.1114873084483,-0.117154521356547,
0.378011969599918));
#16585=CARTESIAN_POINT('Ctrl Pts',(0.0379748391485164,-0.157202141877815,
0.385950959237223));
#16586=CARTESIAN_POINT('Ctrl Pts',(0.152673624090564,-0.0533419752763387,
0.39388994887453));
#16587=CARTESIAN_POINT('Ctrl Pts',(0.127610169584502,0.0993491139263089,
0.401828938511835));
#16588=CARTESIAN_POINT('Ctrl Pts',(-0.014271649480085,0.16109289816887,
0.409767928149142));
#16589=CARTESIAN_POINT('Ctrl Pts',(-0.143088751545671,0.0753671745551693,
0.417706917786446));
#16590=CARTESIAN_POINT('Ctrl Pts',(-0.140917908083783,-0.0793520321139836,
0.425645907423752));
#16591=CARTESIAN_POINT('Ctrl Pts',(-0.00974637750615997,-0.161429891732714,
0.433584897061058));
#16592=CARTESIAN_POINT('Ctrl Pts',(0.130347293715478,-0.0957297489831606,
0.441523886698364));
#16593=CARTESIAN_POINT('Ctrl Pts',(0.15111695082405,0.0576044181723055,
0.449462876335669));
#16594=CARTESIAN_POINT('Ctrl Pts',(0.0335493961742207,0.158205688379633,
0.457401865972975));
#16595=CARTESIAN_POINT('Ctrl Pts',(-0.114730331382826,0.113980493419335,
0.465340855610281));
#16596=CARTESIAN_POINT('Ctrl Pts',(-0.157982303542021,-0.03458603167299,
0.473279845247587));
#16597=CARTESIAN_POINT('Ctrl Pts',(-0.0566123040428622,-0.151491415104245,
0.481218834884892));
#16598=CARTESIAN_POINT('Ctrl Pts',(0.0965823799129518,-0.129716790392294,
0.489157824522198));
#16599=CARTESIAN_POINT('Ctrl Pts',(0.161362514281243,0.0108046658515635,
0.497096814159504));
#16600=CARTESIAN_POINT('Ctrl Pts',(0.0784263257203939,0.141435191000425,
0.50503580379681));
#16601=CARTESIAN_POINT('Ctrl Pts',(-0.076303789130349,0.14259149197508,
0.512974793434115));
#16602=CARTESIAN_POINT('Ctrl Pts',(-0.161183014472451,0.0132150544797126,
0.520913783071421));
#16603=CARTESIAN_POINT('Ctrl Pts',(-0.0985102366584373,-0.128258859705,
0.528852772708727));
#16604=CARTESIAN_POINT('Ctrl Pts',(0.0543419114689404,-0.152320577983508,
0.536791762346032));
#16605=CARTESIAN_POINT('Ctrl Pts',(0.157447763940923,-0.0369432463290883,
0.544730751983338));
#16606=CARTESIAN_POINT('Ctrl Pts',(0.116420979124965,0.112253095453589,
0.552669741620643));
#16607=CARTESIAN_POINT('Ctrl Pts',(-0.0311812332291155,0.158689421555565,
0.56060873125795));
#16608=CARTESIAN_POINT('Ctrl Pts',(-0.150239163551416,0.0598564579197502,
0.568547720895255));
#16609=CARTESIAN_POINT('Ctrl Pts',(-0.131763436204723,-0.0937709907106254,
0.576486710532561));
#16610=CARTESIAN_POINT('Ctrl Pts',(0.00733268664935855,-0.161557523891122,
0.584425700169866));
#16611=CARTESIAN_POINT('Ctrl Pts',(0.139716237417787,-0.0814492162095161,
0.592364689807173));
#16612=CARTESIAN_POINT('Ctrl Pts',(0.144199148209332,0.0732202668325601,
0.600303679444478));
#16613=CARTESIAN_POINT('Ctrl Pts',(0.0166776214282734,0.160861613702037,
0.608242669081784));
#16614=CARTESIAN_POINT('Ctrl Pts',(-0.126111124778327,0.101245177793678,
0.616181658719089));
#16615=CARTESIAN_POINT('Ctrl Pts',(-0.153453779210204,-0.0510542795996006,
0.624120648356396));
#16616=CARTESIAN_POINT('Ctrl Pts',(-0.0403200156494649,-0.156617042997737,
0.6320596379937));
#16617=CARTESIAN_POINT('Ctrl Pts',(0.10972395892722,-0.118807637198397,
0.639998627631007));
#16618=CARTESIAN_POINT('Ctrl Pts',(0.159323168980049,0.0277620180369333,
0.647937617268312));
#16619=CARTESIAN_POINT('Ctrl Pts',(0.0630729369615192,0.148917448414806,
0.655876606905618));
#16620=CARTESIAN_POINT('Ctrl Pts',(-0.0909162461746061,0.133749160748195,
0.663815596542924));
#16621=CARTESIAN_POINT('Ctrl Pts',(-0.161677836835157,-0.00385731715476066,
0.671754586180229));
#16622=CARTESIAN_POINT('Ctrl Pts',(-0.0844344483789265,-0.137932685561743,
0.679693575817536));
#16623=CARTESIAN_POINT('Ctrl Pts',(0.0701028908975481,-0.145740133481257,
0.687632565454841));
#16624=CARTESIAN_POINT('Ctrl Pts',(0.1604658380222,-0.0201324774223393,
0.695571555092147));
#16625=CARTESIAN_POINT('Ctrl Pts',(0.10393330787963,0.123905081947942,0.703510544729453));
#16626=CARTESIAN_POINT('Ctrl Pts',(-0.0477430426119635,0.15451603056473,
0.711449534366758));
#16627=CARTESIAN_POINT('Ctrl Pts',(-0.155713909636705,0.0436781428746717,
0.719388524004064));
#16628=CARTESIAN_POINT('Ctrl Pts',(-0.121139364160222,-0.10714409115852,
0.72732751364137));
#16629=CARTESIAN_POINT('Ctrl Pts',(0.0243299669821161,-0.159883252800214,
0.735266503278675));
#16630=CARTESIAN_POINT('Ctrl Pts',(0.147526880793862,-0.0662602540182413,
0.743205492915981));
#16631=CARTESIAN_POINT('Ctrl Pts',(0.135673045916277,0.0880194662056535,
0.751144482553287));
#16632=CARTESIAN_POINT('Ctrl Pts',(-0.000380164216571841,0.161723397486253,
0.759083472190592));
#16633=CARTESIAN_POINT('Ctrl Pts',(-0.136085360063504,0.0873806419964673,
0.767022461827899));
#16634=CARTESIAN_POINT('Ctrl Pts',(-0.147213735311121,-0.0669531026545853,
0.774961451465203));
#16635=CARTESIAN_POINT('Ctrl Pts',(-0.023578025097595,-0.159995870421162,
0.78290044110251));
#16636=CARTESIAN_POINT('Ctrl Pts',(0.121641751185188,-0.106573384050283,
0.790839430739816));
#16637=CARTESIAN_POINT('Ctrl Pts',(0.155506840911589,0.0444097314676148,
0.798778420377121));
#16638=CARTESIAN_POINT('Ctrl Pts',(0.047016075363265,0.15473878142458,0.806717410014428));
#16639=CARTESIAN_POINT('Ctrl Pts',(-0.104514684958047,0.123415081928621,
0.814656399651731));
#16640=CARTESIAN_POINT('Ctrl Pts',(-0.16036941405942,-0.020886666885039,
0.82259538928904));
#16641=CARTESIAN_POINT('Ctrl Pts',(-0.0694169354231278,-0.146068103622213,
0.830534378926343));
#16642=CARTESIAN_POINT('Ctrl Pts',(0.085081990139753,-0.137534202194171,
0.838473368563651));
#16643=CARTESIAN_POINT('Ctrl Pts',(0.161694184779289,-0.00309716449182502,
0.846412358200955));
#16644=CARTESIAN_POINT('Ctrl Pts',(0.0902864348795877,0.134175115040242,
0.854351347838261));
#16645=CARTESIAN_POINT('Ctrl Pts',(-0.0637723584188847,0.148619272374149,
0.862290337475567));
#16646=CARTESIAN_POINT('Ctrl Pts',(-0.159451928190027,0.0270126713934565,
0.870229327112872));
#16647=CARTESIAN_POINT('Ctrl Pts',(-0.109164185657521,-0.119322178948671,
0.878168316750179));
#16648=CARTESIAN_POINT('Ctrl Pts',(0.0410558873341998,-0.156425752146281,
0.886107306387484));
#16649=CARTESIAN_POINT('Ctrl Pts',(0.153692109215179,-0.0503322698109037,
0.894046296024789));
#16650=CARTESIAN_POINT('Ctrl Pts',(0.125633738317809,0.101836956040625,
0.901985285662096));
#16651=CARTESIAN_POINT('Ctrl Pts',(-0.0174337097671096,0.160781427979367,
0.909924275299401));
#16652=CARTESIAN_POINT('Ctrl Pts',(-0.144541791370401,0.072541521673891,
0.917863264936708));
#16653=CARTESIAN_POINT('Ctrl Pts',(-0.13933176907,-0.082105176128868,0.925802254574012));
#16654=CARTESIAN_POINT('Ctrl Pts',(-0.00657306121577474,-0.161590212220858,
0.933741244211319));
#16655=CARTESIAN_POINT('Ctrl Pts',(0.132202833700187,-0.0931504835251481,
0.941680233848624));
#16656=CARTESIAN_POINT('Ctrl Pts',(0.149956094815541,0.0605621288182698,
0.949619223485929));
#16657=CARTESIAN_POINT('Ctrl Pts',(0.0304348282896272,0.158834262822317,
0.957558213123236));
#16658=CARTESIAN_POINT('Ctrl Pts',(-0.116947437700435,0.111704514835484,
0.965497202760542));
#16659=CARTESIAN_POINT('Ctrl Pts',(-0.157272339407096,-0.0376830608728604,
0.973436192397847));
#16660=CARTESIAN_POINT('Ctrl Pts',(-0.0536251929639052,-0.152574376940928,
0.981375182035153));
#16661=CARTESIAN_POINT('Ctrl Pts',(0.0991121424632477,-0.127794307524525,
0.989314171672459));
#16662=CARTESIAN_POINT('Ctrl Pts',(0.161119104064031,0.0139726921146952,
0.997253161309763));
#16663=CARTESIAN_POINT('Ctrl Pts',(0.0756325681075411,0.142948649734045,
1.00519215094707));
#16664=CARTESIAN_POINT('Ctrl Pts',(-0.0790904005129918,0.141064915432658,
1.01313114058437));
#16665=CARTESIAN_POINT('Ctrl Pts',(-0.161411527883023,0.0100459188627121,
1.02107013022168));
#16666=CARTESIAN_POINT('Ctrl Pts',(-0.095971463730607,-0.130169427934261,
1.02900911985899));
#16667=CARTESIAN_POINT('Ctrl Pts',(0.0573238981132153,-0.151223584550935,
1.03694810949629));
#16668=CARTESIAN_POINT('Ctrl Pts',(0.158143159897702,-0.0338429135403315,
1.0448870991336));
#16669=CARTESIAN_POINT('Ctrl Pts',(0.114193197054413,0.114518625410106,
1.0528260887709));
#16670=CARTESIAN_POINT('Ctrl Pts',(-0.0342928115212847,0.158046211271557,
1.06076507840821));
#16671=CARTESIAN_POINT('Ctrl Pts',(-0.151386101389109,0.0568933223281485,
1.06870406804552));
#16672=CARTESIAN_POINT('Ctrl Pts',(-0.129895790602315,-0.0963415040526547,
1.07664305768282));
#16673=CARTESIAN_POINT('Ctrl Pts',(0.0105052141409744,-0.161382286187737,
1.08458204732013));
#16674=CARTESIAN_POINT('Ctrl Pts',(0.141289415307547,-0.0786886455683398,
1.09252103695743));
#16675=CARTESIAN_POINT('Ctrl Pts',(0.14273283995608,0.076039057183793,1.10046002659474));
#16676=CARTESIAN_POINT('Ctrl Pts',(0.013514131745196,0.161158214381091,
1.10839901623204));
#16677=CARTESIAN_POINT('Ctrl Pts',(-0.128075837894479,0.0987480712062529,
1.11633800586935));
#16678=CARTESIAN_POINT('Ctrl Pts',(-0.152421155552179,-0.0540591635106084,
1.12427699550666));
#16679=CARTESIAN_POINT('Ctrl Pts',(-0.0372353514058616,-0.157378938949945,
1.13221598514396));
#16680=CARTESIAN_POINT('Ctrl Pts',(0.11203686504723,-0.116629081663695,
1.14015497478127));
#16681=CARTESIAN_POINT('Ctrl Pts',(0.158747009937404,0.0308867067726846,
1.14809396441857));
#16682=CARTESIAN_POINT('Ctrl Pts',(0.0601351468730053,0.150127831962932,
1.15603295405588));
#16683=CARTESIAN_POINT('Ctrl Pts',(-0.0935263218228598,0.13193721592339,
1.16397194369318));
#16684=CARTESIAN_POINT('Ctrl Pts',(-0.161570852667341,-0.00703287904607843,
1.17191093333049));
#16685=CARTESIAN_POINT('Ctrl Pts',(-0.0817083410685703,-0.13956485524354,
1.17984992296779));
#16686=CARTESIAN_POINT('Ctrl Pts',(0.0729525569401478,-0.144334771469742,
1.1877889126051));
#16687=CARTESIAN_POINT('Ctrl Pts',(0.160830388835411,-0.016976096323307,
1.19572790224241));
#16688=CARTESIAN_POINT('Ctrl Pts',(0.101479022178261,0.125923031559255,
1.20366689187971));
#16689=CARTESIAN_POINT('Ctrl Pts',(-0.0507694344715009,0.153548254118279,
1.21160588151702));
#16690=CARTESIAN_POINT('Ctrl Pts',(-0.15654195331917,0.0406105733811438,
1.21954487115432));
#16691=CARTESIAN_POINT('Ctrl Pts',(-0.119011042423884,-0.109503304062093,
1.22748386079163));
#16692=CARTESIAN_POINT('Ctrl Pts',(0.0274663214511058,-0.159374411387982,
1.23542285042894));
#16693=CARTESIAN_POINT('Ctrl Pts',(0.148800150427453,-0.0633491677300162,
1.24336184006624));
#16694=CARTESIAN_POINT('Ctrl Pts',(0.133917639627974,0.0906678973829495,
1.25130082970354));
#16695=CARTESIAN_POINT('Ctrl Pts',(-0.00355729227603857,0.161684716318317,
1.25923981934086));
#16696=CARTESIAN_POINT('Ctrl Pts',(-0.137775766897813,0.0846902584421788,
1.26717880897816));
#16697=CARTESIAN_POINT('Ctrl Pts',(-0.14586996931591,-0.0698323268364953,
1.27511779861547));
#16698=CARTESIAN_POINT('Ctrl Pts',(-0.0204302119447119,-0.160428202816007,
1.28305678825277));
#16699=CARTESIAN_POINT('Ctrl Pts',(0.123712004283314,-0.104163053984564,
1.29099577789008));
#16700=CARTESIAN_POINT('Ctrl Pts',(0.15460435913624,0.0474562320176185,
1.29893476752738));
#16701=CARTESIAN_POINT('Ctrl Pts',(0.043967018911749,0.155632589980133,
1.30687375716469));
#16702=CARTESIAN_POINT('Ctrl Pts',(-0.106919113837756,0.121337978043289,
1.31481274680199));
#16703=CARTESIAN_POINT('Ctrl Pts',(-0.159928125575155,-0.0240332370134145,
1.3227517364393));
#16704=CARTESIAN_POINT('Ctrl Pts',(-0.0665338988230771,-0.147403670583407,
1.33069072607661));
#16705=CARTESIAN_POINT('Ctrl Pts',(0.0877675522160205,-0.135836146169277,
1.33862971571391));
#16706=CARTESIAN_POINT('Ctrl Pts',(0.161723824721502,8.00609866524728E-5,
1.34656870535122));
#16707=CARTESIAN_POINT('Ctrl Pts',(0.0876330185603928,0.135922977069285,
1.35450769498852));
#16708=CARTESIAN_POINT('Ctrl Pts',(-0.0666798087068602,0.147337724435113,
1.36244668462583));
#16709=CARTESIAN_POINT('Ctrl Pts',(-0.159951843822013,0.0238748801740983,
1.37038567426313));
#16710=CARTESIAN_POINT('Ctrl Pts',(-0.106798922716859,-0.121443775659372,
1.37832466390044));
#16711=CARTESIAN_POINT('Ctrl Pts',(0.0441210824430389,-0.155588987406456,
1.38626365353774));
#16712=CARTESIAN_POINT('Ctrl Pts',(0.154651279966657,-0.0473031264624986,
1.39420264317505));
#16713=CARTESIAN_POINT('Ctrl Pts',(0.123608792556459,0.10428547082216,1.40214163281236));
#16714=CARTESIAN_POINT('Ctrl Pts',(-0.020589002599541,0.160407931346284,
1.41008062244966));
#16715=CARTESIAN_POINT('Ctrl Pts',(-0.145939110542184,0.0696878015005003,
1.41801961208697));
#16716=CARTESIAN_POINT('Ctrl Pts',(-0.137691710982408,-0.0848265016612731,
1.42595860172427));
#16717=CARTESIAN_POINT('Ctrl Pts',(-0.00339746822928561,-0.161688398335044,
1.43389759136158));
#16718=CARTESIAN_POINT('Ctrl Pts',(0.134007838137522,-0.0905348079547059,
1.44183658099889));
#16719=CARTESIAN_POINT('Ctrl Pts',(0.148736417039967,0.0634956003383226,
1.44977557063619));
#16720=CARTESIAN_POINT('Ctrl Pts',(0.0273102951854726,0.159403164432859,
1.4577145602735));
#16721=CARTESIAN_POINT('Ctrl Pts',(-0.119122786779006,0.109382310628272,
1.4656535499108));
#16722=CARTESIAN_POINT('Ctrl Pts',(-0.156495242883694,-0.0407596439572756,
1.47359253954811));
#16723=CARTESIAN_POINT('Ctrl Pts',(-0.0506295842364637,-0.153609649276743,
1.48153152918541));
#16724=CARTESIAN_POINT('Ctrl Pts',(0.10162683549218,-0.125801210382132,
1.48947051882272));
#16725=CARTESIAN_POINT('Ctrl Pts',(0.160769288057966,0.017094787472962,
1.49740950846002));
#16726=CARTESIAN_POINT('Ctrl Pts',(0.0728951834924312,0.144484958595688,
1.50534849809733));
#16727=CARTESIAN_POINT('Ctrl Pts',(-0.0820226078184241,0.139326700971572,
1.51328748773464));
#16728=CARTESIAN_POINT('Ctrl Pts',(-0.134767702434085,0.0512744806661359,
1.51858014749284));
#16729=CARTESIAN_POINT('Ctrl Pts',(-0.136701386950156,0.00581475974600206,
1.52122647737194));
#16730=CARTESIAN_POINT('Ctrl Pts',(0.0740036351041134,-0.103579689087085,
-0.0054992613140312));
#16731=CARTESIAN_POINT('Ctrl Pts',(0.108448814220036,-0.0789699563406641,
-0.00285293143492929));
#16732=CARTESIAN_POINT('Ctrl Pts',(0.150264871169078,0.00688399744800666,
0.00243972832327453));
#16733=CARTESIAN_POINT('Ctrl Pts',(0.0755551489391376,0.130236700260234,
0.0103787179605803));
#16734=CARTESIAN_POINT('Ctrl Pts',(-0.0683810376584167,0.133979098529349,
0.0183177075978859));
#16735=CARTESIAN_POINT('Ctrl Pts',(-0.14968704878538,0.0152677557027674,
0.0262566972351917));
#16736=CARTESIAN_POINT('Ctrl Pts',(-0.0939816891590436,-0.11752176362514,
0.0341956868724974));
#16737=CARTESIAN_POINT('Ctrl Pts',(0.0477663481097245,-0.142674779628989,
0.0421346765098031));
#16738=CARTESIAN_POINT('Ctrl Pts',(0.14578288888032,-0.0372469160898187,
0.0500736661471088));
#16739=CARTESIAN_POINT('Ctrl Pts',(0.110347650287512,0.102292747252513,
0.0580126557844146));
#16740=CARTESIAN_POINT('Ctrl Pts',(-0.0261045975097209,0.148182615303324,
0.0659516454217203));
#16741=CARTESIAN_POINT('Ctrl Pts',(-0.13865919166998,0.0584255608647477,
0.073890635059026));
#16742=CARTESIAN_POINT('Ctrl Pts',(-0.124281158904105,-0.0848182532198701,
0.0818296246963318));
#16743=CARTESIAN_POINT('Ctrl Pts',(0.00386794697500161,-0.15041563023346,
0.0897686143336374));
#16744=CARTESIAN_POINT('Ctrl Pts',(0.128476112576568,-0.0783184064825255,
0.0977076039709433));
#16745=CARTESIAN_POINT('Ctrl Pts',(0.135473254782295,0.0654742669580799,
0.105646593608249));
#16746=CARTESIAN_POINT('Ctrl Pts',(0.0184538891044151,0.149329569763132,
0.113585583245555));
#16747=CARTESIAN_POINT('Ctrl Pts',(-0.115458732720671,0.096483973363118,
0.12152457288286));
#16748=CARTESIAN_POINT('Ctrl Pts',(-0.143676805334049,-0.0446861343604874,
0.129463562520166));
#16749=CARTESIAN_POINT('Ctrl Pts',(-0.0403686054279526,-0.144949124289353,
0.137402552157472));
#16750=CARTESIAN_POINT('Ctrl Pts',(0.0998942839726139,-0.112521137758025,
0.145341541794778));
#16751=CARTESIAN_POINT('Ctrl Pts',(0.14871080372247,0.0229122455632766,
0.153280531432083));
#16752=CARTESIAN_POINT('Ctrl Pts',(0.0613927738894439,0.137371034794898,
0.161219521069389));
#16753=CARTESIAN_POINT('Ctrl Pts',(-0.0821261326059948,0.126076058196294,
0.169158510706695));
#16754=CARTESIAN_POINT('Ctrl Pts',(-0.150464193336327,-0.000632910110818063,
0.177097500344));
#16755=CARTESIAN_POINT('Ctrl Pts',(-0.0810625969653723,-0.126762492068094,
0.185036489981306));
#16756=CARTESIAN_POINT('Ctrl Pts',(0.0625462512992226,-0.136849700411639,
0.192975479618612));
#16757=CARTESIAN_POINT('Ctrl Pts',(0.148898293097928,-0.0216603868066741,
0.200914469255917));
#16758=CARTESIAN_POINT('Ctrl Pts',(0.0989441522193119,0.113357526360621,
0.208853458893223));
#16759=CARTESIAN_POINT('Ctrl Pts',(-0.0415865789238149,0.144604393083411,
0.216792448530529));
#16760=CARTESIAN_POINT('Ctrl Pts',(-0.144047647180085,0.0434758483035601,
0.224731438167835));
#16761=CARTESIAN_POINT('Ctrl Pts',(-0.114642966671137,-0.0974518559926297,
0.232670427805141));
#16762=CARTESIAN_POINT('Ctrl Pts',(0.0197094928286333,-0.149169064945282,
0.240609417442446));
#16763=CARTESIAN_POINT('Ctrl Pts',(0.136019262424063,-0.0643322181611298,
0.248548407079752));
#16764=CARTESIAN_POINT('Ctrl Pts',(0.127812719278849,0.0793963653730636,
0.256487396717058));
#16765=CARTESIAN_POINT('Ctrl Pts',(0.00260239121171357,0.150443017797356,
0.264426386354363));
#16766=CARTESIAN_POINT('Ctrl Pts',(-0.124990247656303,0.0837693979610897,
0.272365375991669));
#16767=CARTESIAN_POINT('Ctrl Pts',(-0.138162880936044,-0.0595893646165358,
0.280304365628975));
#16768=CARTESIAN_POINT('Ctrl Pts',(-0.0248568656394851,-0.148398147813718,
0.288243355266281));
#16769=CARTESIAN_POINT('Ctrl Pts',(0.111203906597776,-0.101358597076653,
0.296182344903586));
#16770=CARTESIAN_POINT('Ctrl Pts',(0.145465123646218,0.0384678027257296,
0.304121334540892));
#16771=CARTESIAN_POINT('Ctrl Pts',(0.0465629893725541,0.143079565503422,
0.312060324178198));
#16772=CARTESIAN_POINT('Ctrl Pts',(-0.0949643705016135,0.116711791945748,
0.319999313815503));
#16773=CARTESIAN_POINT('Ctrl Pts',(-0.149558357514911,-0.0164976283567656,
0.327938303452809));
#16774=CARTESIAN_POINT('Ctrl Pts',(-0.0672419181269484,-0.134604600554976,
0.335877293090115));
#16775=CARTESIAN_POINT('Ctrl Pts',(0.0766298889166206,-0.12949028600085,
0.343816282727421));
#16776=CARTESIAN_POINT('Ctrl Pts',(0.150352284446295,-0.00583648916182633,
0.351755272364726));
#16777=CARTESIAN_POINT('Ctrl Pts',(0.0864374678803939,0.123160213504125,
0.359694262002032));
#16778=CARTESIAN_POINT('Ctrl Pts',(-0.0566049265834532,0.139412181427728,
0.367633251639338));
#16779=CARTESIAN_POINT('Ctrl Pts',(-0.147829390149123,0.0280418517950267,
0.375572241276644));
#16780=CARTESIAN_POINT('Ctrl Pts',(-0.103726178443039,-0.108998871322406,
0.383511230913949));
#16781=CARTESIAN_POINT('Ctrl Pts',(0.0353312408083745,-0.146258597924691,
0.391450220551255));
#16782=CARTESIAN_POINT('Ctrl Pts',(0.142045330507792,-0.0496286018832686,
0.399389210188561));
#16783=CARTESIAN_POINT('Ctrl Pts',(0.118726655129599,0.0924329779120693,
0.407328199825866));
#16784=CARTESIAN_POINT('Ctrl Pts',(-0.0132781361506635,0.1498785012746,
0.415267189463172));
#16785=CARTESIAN_POINT('Ctrl Pts',(-0.133127703795094,0.0701205285647604,
0.423206179100478));
#16786=CARTESIAN_POINT('Ctrl Pts',(-0.131107982452518,-0.0738279823724454,
0.431145168737783));
#16787=CARTESIAN_POINT('Ctrl Pts',(-0.00906788859151817,-0.150192035209753,
0.439084158375089));
#16788=CARTESIAN_POINT('Ctrl Pts',(0.121273235812024,-0.0890655731449414,
0.447023148012395));
#16789=CARTESIAN_POINT('Ctrl Pts',(0.14059702422731,0.0535943170716914,
0.4549621376497));
#16790=CARTESIAN_POINT('Ctrl Pts',(0.031213872705855,0.14719228306762,0.462901127287006));
#16791=CARTESIAN_POINT('Ctrl Pts',(-0.106743440051405,0.106045801661112,
0.470840116924312));
#16792=CARTESIAN_POINT('Ctrl Pts',(-0.146984449047318,-0.0321783433727119,
0.478779106561618));
#16793=CARTESIAN_POINT('Ctrl Pts',(-0.0526712684425847,-0.140945420374714,
0.486718096198923));
#16794=CARTESIAN_POINT('Ctrl Pts',(0.0898588486235595,-0.120686624644175,
0.49465708583623));
#16795=CARTESIAN_POINT('Ctrl Pts',(0.150129348203927,0.0100525047535443,
0.502596075473534));
#16796=CARTESIAN_POINT('Ctrl Pts',(0.0729667185397875,0.131589254992538,
0.510535065110842));
#16797=CARTESIAN_POINT('Ctrl Pts',(-0.0709919412117167,0.132665060686482,
0.518474054748145));
#16798=CARTESIAN_POINT('Ctrl Pts',(-0.149962344179375,0.0122950954523496,
0.526413044385453));
#16799=CARTESIAN_POINT('Ctrl Pts',(-0.0916524986414713,-0.119330187030486,
0.534352034022757));
#16800=CARTESIAN_POINT('Ctrl Pts',(0.0505589280467443,-0.141716861518734,
0.542291023660064));
#16801=CARTESIAN_POINT('Ctrl Pts',(0.146487121137799,-0.0343714617774037,
0.550230013297369));
#16802=CARTESIAN_POINT('Ctrl Pts',(0.108316394245265,0.104438655591022,
0.558169002934674));
#16803=CARTESIAN_POINT('Ctrl Pts',(-0.0290105681715044,0.147642341414387,
0.566107992571982));
#16804=CARTESIAN_POINT('Ctrl Pts',(-0.139780343651344,0.0556895822633619,
0.574046982209285));
#16805=CARTESIAN_POINT('Ctrl Pts',(-0.122590794290966,-0.0872431727934394,
0.581985971846593));
#16806=CARTESIAN_POINT('Ctrl Pts',(0.00682222554696161,-0.150310782322966,
0.589924961483898));
#16807=CARTESIAN_POINT('Ctrl Pts',(0.129989965454297,-0.0757791721064987,
0.597863951121203));
#16808=CARTESIAN_POINT('Ctrl Pts',(0.134160800782372,0.0681230766876274,
0.60580294075851));
#16809=CARTESIAN_POINT('Ctrl Pts',(0.015516617634347,0.149663317553585,
0.613741930395814));
#16810=CARTESIAN_POINT('Ctrl Pts',(-0.117331965534667,0.0941970482962578,
0.621680920033121));
#16811=CARTESIAN_POINT('Ctrl Pts',(-0.142771175541451,-0.0475001629309618,
0.629619909670426));
#16812=CARTESIAN_POINT('Ctrl Pts',(-0.0375131590877193,-0.145714230393655,
0.637558899307733));
#16813=CARTESIAN_POINT('Ctrl Pts',(0.102085583566124,-0.110536906379362,
0.645497888945037));
#16814=CARTESIAN_POINT('Ctrl Pts',(0.148231970847143,0.0258293798362968,
0.653436878582344));
#16815=CARTESIAN_POINT('Ctrl Pts',(0.0586821478180281,0.138550639014834,
0.661375868219649));
#16816=CARTESIAN_POINT('Ctrl Pts',(-0.0845871597882484,0.124438283670714,
0.669314857856955));
#16817=CARTESIAN_POINT('Ctrl Pts',(-0.150422719745043,-0.00358879206139753,
0.67725384749426));
#16818=CARTESIAN_POINT('Ctrl Pts',(-0.078556588917505,-0.128330574617282,
0.685192837131567));
#16819=CARTESIAN_POINT('Ctrl Pts',(0.065222715229363,-0.135594511179713,
0.693131826768872));
#16820=CARTESIAN_POINT('Ctrl Pts',(0.149295093588351,-0.0187309656558678,
0.701070816406178));
#16821=CARTESIAN_POINT('Ctrl Pts',(0.0966980456281902,0.11527949520901,
0.709009806043483));
#16822=CARTESIAN_POINT('Ctrl Pts',(-0.044419435954706,0.14375947882982,
0.716948795680789));
#16823=CARTESIAN_POINT('Ctrl Pts',(-0.144873968183829,0.0406375120624596,
0.724887785318095));
#16824=CARTESIAN_POINT('Ctrl Pts',(-0.112706311402131,-0.099685311927494,
0.732826774955401));
#16825=CARTESIAN_POINT('Ctrl Pts',(0.0226362492002416,-0.148753064728429,
0.740765764592706));
#16826=CARTESIAN_POINT('Ctrl Pts',(0.137256875023267,-0.0616475814838108,
0.748704754230013));
#16827=CARTESIAN_POINT('Ctrl Pts',(0.126228238590478,0.0818920376245527,
0.756643743867318));
#16828=CARTESIAN_POINT('Ctrl Pts',(-0.000353699285724532,0.150465108715513,
0.764582733504624));
#16829=CARTESIAN_POINT('Ctrl Pts',(-0.126611849706441,0.0812976848247803,
0.772521723141928));
#16830=CARTESIAN_POINT('Ctrl Pts',(-0.136965528997667,-0.0622921978288208,
0.780460712779236));
#16831=CARTESIAN_POINT('Ctrl Pts',(-0.0219366533522686,-0.148857842533265,
0.788399702416541));
#16832=CARTESIAN_POINT('Ctrl Pts',(0.113173725020093,-0.0991543342927188,
0.796338692053846));
#16833=CARTESIAN_POINT('Ctrl Pts',(0.144681314438483,0.0413181715024817,
0.804277681691154));
#16834=CARTESIAN_POINT('Ctrl Pts',(0.0437430761464933,0.143966723006387,
0.812216671328456));
#16835=CARTESIAN_POINT('Ctrl Pts',(-0.0972389504488157,0.114823606281847,
0.820155660965765));
#16836=CARTESIAN_POINT('Ctrl Pts',(-0.149205382128735,-0.0194326526180533,
0.828094650603069));
#16837=CARTESIAN_POINT('Ctrl Pts',(-0.0645845121824554,-0.135899649852787,
0.836033640240376));
#16838=CARTESIAN_POINT('Ctrl Pts',(0.0791590524011713,-0.127959831458565,
0.843972629877681));
#16839=CARTESIAN_POINT('Ctrl Pts',(0.150437929635691,-0.00288155702400619,
0.851911619514986));
#16840=CARTESIAN_POINT('Ctrl Pts',(0.0840011924733913,0.12483458538003,
0.859850609152293));
#16841=CARTESIAN_POINT('Ctrl Pts',(-0.0593328794206009,0.138273220341526,
0.867789598789597));
#16842=CARTESIAN_POINT('Ctrl Pts',(-0.148351766552825,0.0251321985630355,
0.875728588426904));
#16843=CARTESIAN_POINT('Ctrl Pts',(-0.1015647786165,-0.111015628577859,
0.883667578064211));
#16844=CARTESIAN_POINT('Ctrl Pts',(0.0381978034543637,-0.145536256153639,
0.891606567701514));
#16845=CARTESIAN_POINT('Ctrl Pts',(0.142992914329196,-0.046828415471795,
0.899545557338823));
#16846=CARTESIAN_POINT('Ctrl Pts',(0.116887812080083,0.0947476302135675,
0.907484546976125));
#16847=CARTESIAN_POINT('Ctrl Pts',(-0.0162200712834111,0.149588713917584,
0.915423536613434));
#16848=CARTESIAN_POINT('Ctrl Pts',(-0.134479591021026,0.067491582014154,
0.923362526250738));
#16849=CARTESIAN_POINT('Ctrl Pts',(-0.129632261667175,-0.0763894677230377,
0.931301515888044));
#16850=CARTESIAN_POINT('Ctrl Pts',(-0.00611548103612966,-0.150341195071919,
0.93924050552535));
#16851=CARTESIAN_POINT('Ctrl Pts',(0.122999603362204,-0.0866658618874593,
0.947179495162656));
#16852=CARTESIAN_POINT('Ctrl Pts',(0.139516980595786,0.0563461282555487,
0.95511848479996));
#16853=CARTESIAN_POINT('Ctrl Pts',(0.0283161238170646,0.147777099632969,
0.963057474437267));
#16854=CARTESIAN_POINT('Ctrl Pts',(-0.108806203685475,0.103928264122473,
0.970996464074573));
#16855=CARTESIAN_POINT('Ctrl Pts',(-0.146323908690103,-0.0350597745230392,
0.978935453711877));
#16856=CARTESIAN_POINT('Ctrl Pts',(-0.049892103521326,-0.14195299239598,
0.986874443349185));
#16857=CARTESIAN_POINT('Ctrl Pts',(0.0922125030920605,-0.118897974404329,
0.994813432986488));
#16858=CARTESIAN_POINT('Ctrl Pts',(0.149902882860231,0.0129999905441286,
1.0027524226238));
#16859=CARTESIAN_POINT('Ctrl Pts',(0.0703674468853664,0.132997355096976,
1.0106914122611));
#16860=CARTESIAN_POINT('Ctrl Pts',(-0.0735845641169637,0.131244755962562,
1.01863040189841));
#16861=CARTESIAN_POINT('Ctrl Pts',(-0.150174949749745,0.00934657753497952,
1.02656939153571));
#16862=CARTESIAN_POINT('Ctrl Pts',(-0.0892904610481016,-0.121107752063083,
1.03450838117302));
#16863=CARTESIAN_POINT('Ctrl Pts',(0.0533333252681307,-0.140696234703703,
1.04244737081032));
#16864=CARTESIAN_POINT('Ctrl Pts',(0.147134107472884,-0.031486957015783,
1.05038636044763));
#16865=CARTESIAN_POINT('Ctrl Pts',(0.106243698045146,0.106546471877992,
1.05832535008494));
#16866=CARTESIAN_POINT('Ctrl Pts',(-0.0319055355867657,0.147043907874068,
1.06626433972224));
#16867=CARTESIAN_POINT('Ctrl Pts',(-0.14084743801815,0.0529327237885883,
1.07420332935955));
#16868=CARTESIAN_POINT('Ctrl Pts',(-0.120853163849259,-0.0896347412088629,
1.08214231899685));
#16869=CARTESIAN_POINT('Ctrl Pts',(0.00977389921538986,-0.150147743699608,
1.09008130863416));
#16870=CARTESIAN_POINT('Ctrl Pts',(0.13145362739741,-0.0732107771302755,
1.09802029827146));
#16871=CARTESIAN_POINT('Ctrl Pts',(0.132796568802552,0.0707456384395876,
1.10595928790877));
#16872=CARTESIAN_POINT('Ctrl Pts',(0.0125733526121963,0.149939270533256,
1.11389827754607));
#16873=CARTESIAN_POINT('Ctrl Pts',(-0.119159906186493,0.0918737764630459,
1.12183726718338));
#16874=CARTESIAN_POINT('Ctrl Pts',(-0.141810437433163,-0.0502958634379693,
1.12977625682069));
#16875=CARTESIAN_POINT('Ctrl Pts',(-0.0346432321137694,-0.146423087362162,
1.13771524645799));
#16876=CARTESIAN_POINT('Ctrl Pts',(0.104237477950025,-0.108510009835838,
1.1456542360953));
#16877=CARTESIAN_POINT('Ctrl Pts',(0.147695920811486,0.0287365450185451,
1.1535932257326));
#16878=CARTESIAN_POINT('Ctrl Pts',(0.0559488704325515,0.139676762352502,
1.16153221536991));
#16879=CARTESIAN_POINT('Ctrl Pts',(-0.0870155364008756,0.12275247642644,
1.16947120500722));
#16880=CARTESIAN_POINT('Ctrl Pts',(-0.150323183223479,-0.00654328889139735,
1.17741019464452));
#16881=CARTESIAN_POINT('Ctrl Pts',(-0.0760202581255566,-0.129849121670035,
1.18534918428183));
#16882=CARTESIAN_POINT('Ctrl Pts',(0.0678740032777675,-0.134286982701248,
1.19328817391913));
#16883=CARTESIAN_POINT('Ctrl Pts',(0.149634266389533,-0.0157943143574443,
1.20122716355644));
#16884=CARTESIAN_POINT('Ctrl Pts',(0.0944146137277022,0.117156966325547,
1.20916615319374));
#16885=CARTESIAN_POINT('Ctrl Pts',(-0.047235147145783,0.142859073628774,
1.21710514283105));
#16886=CARTESIAN_POINT('Ctrl Pts',(-0.145644368043342,0.037783489796601,
1.22504413246835));
#16887=CARTESIAN_POINT('Ctrl Pts',(-0.11072615165767,-0.101880289472715,
1.23298312210566));
#16888=CARTESIAN_POINT('Ctrl Pts',(0.0255542680118797,-0.148279646041953,
1.24092211174296));
#16889=CARTESIAN_POINT('Ctrl Pts',(0.138441506664824,-0.0589391489276913,
1.24886110138027));
#16890=CARTESIAN_POINT('Ctrl Pts',(0.124595033982396,0.0843560996663564,
1.25680009101758));
#16891=CARTESIAN_POINT('Ctrl Pts',(-0.00330965325590636,0.150429120316621,
1.26473908065488));
#16892=CARTESIAN_POINT('Ctrl Pts',(-0.128184579763139,0.0787945908985174,
1.27267807029219));
#16893=CARTESIAN_POINT('Ctrl Pts',(-0.135715308561414,-0.0649709863423027,
1.2806170599295));
#16894=CARTESIAN_POINT('Ctrl Pts',(-0.0190079735469551,-0.149260078337129,
1.2885560495668));
#16895=CARTESIAN_POINT('Ctrl Pts',(0.115099858543875,-0.0969117980795561,
1.29649503920411));
#16896=CARTESIAN_POINT('Ctrl Pts',(0.143841658454547,0.0441525915281748,
1.30443402884141));
#16897=CARTESIAN_POINT('Ctrl Pts',(0.0409062781470196,0.144798309552134,
1.31237301847872));
#16898=CARTESIAN_POINT('Ctrl Pts',(-0.0994759962839106,0.112891098884786,
1.32031200811602));
#16899=CARTESIAN_POINT('Ctrl Pts',(-0.148794813708878,-0.0223601759313527,
1.32825099775333));
#16900=CARTESIAN_POINT('Ctrl Pts',(-0.0619021766503053,-0.13714224202644,
1.33618998739064));
#16901=CARTESIAN_POINT('Ctrl Pts',(0.0816576604940555,-0.126379984705639,
1.34412897702794));
#16902=CARTESIAN_POINT('Ctrl Pts',(0.150465506209006,7.4487583413377E-5,
1.35206796666525));
#16903=CARTESIAN_POINT('Ctrl Pts',(0.0815324923277053,0.126460770918471,
1.36000695630255));
#16904=CARTESIAN_POINT('Ctrl Pts',(-0.062037929094705,0.137080886684378,
1.36794594593986));
#16905=CARTESIAN_POINT('Ctrl Pts',(-0.148816880822527,0.0222128430196456,
1.37588493557716));
#16906=CARTESIAN_POINT('Ctrl Pts',(-0.0993641722043223,-0.112989531455785,
1.38382392521447));
#16907=CARTESIAN_POINT('Ctrl Pts',(0.0410496166270677,-0.144757742348562,
1.39176291485178));
#16908=CARTESIAN_POINT('Ctrl Pts',(0.143885312916173,-0.0440101443352923,
1.39970190448908));
#16909=CARTESIAN_POINT('Ctrl Pts',(0.115003831846793,0.0970256929337524,
1.40764089412639));
#16910=CARTESIAN_POINT('Ctrl Pts',(-0.0191557100743377,0.149241218055048,
1.41557988376369));
#16911=CARTESIAN_POINT('Ctrl Pts',(-0.135779636557791,0.0648365220611291,
1.423518873401));
#16912=CARTESIAN_POINT('Ctrl Pts',(-0.128106375355825,-0.0789213496179777,
1.4314578630383));
#16913=CARTESIAN_POINT('Ctrl Pts',(-0.00316095527563228,-0.150432546011701,
1.43939685267561));
#16914=CARTESIAN_POINT('Ctrl Pts',(0.12467895337041,-0.0842322751882648,
1.44733584231291));
#16915=CARTESIAN_POINT('Ctrl Pts',(0.138382210043398,0.0590753877074232,
1.45527483195022));
#16916=CARTESIAN_POINT('Ctrl Pts',(0.0254091034322018,0.148306397458819,
1.46321382158753));
#16917=CARTESIAN_POINT('Ctrl Pts',(-0.110830116988615,0.101767718932792,
1.47115281122483));
#16918=CARTESIAN_POINT('Ctrl Pts',(-0.145600909330124,-0.0379221829034233,
1.47909180086214));
#16919=CARTESIAN_POINT('Ctrl Pts',(-0.0471050325108872,-0.142916194795756,
1.48703079049945));
#16920=CARTESIAN_POINT('Ctrl Pts',(0.0945521370959566,-0.117043625665234,
1.49496978013675));
#16921=CARTESIAN_POINT('Ctrl Pts',(0.14957741911039,0.0159047428854941,
1.50290876977406));
#16922=CARTESIAN_POINT('Ctrl Pts',(0.0678206238522695,0.134426714629862,
1.51084775941136));
#16923=CARTESIAN_POINT('Ctrl Pts',(-0.0763126473618499,0.129627546381738,
1.51878674904867));
#16924=CARTESIAN_POINT('Ctrl Pts',(-0.125385920115907,0.0477050348167321,
1.52407940880687));
#16925=CARTESIAN_POINT('Ctrl Pts',(-0.127184992207234,0.00540996832206346,
1.52672573868597));
#16926=CARTESIAN_POINT('Ctrl Pts',(0.0684664424539414,-0.095829519891843,
-1.38777878078145E-17));
#16927=CARTESIAN_POINT('Ctrl Pts',(0.100334321247169,-0.0730611673843044,
0.00264632987910189));
#16928=CARTESIAN_POINT('Ctrl Pts',(0.139021564822767,0.00636891437108143,
0.00793898963730573));
#16929=CARTESIAN_POINT('Ctrl Pts',(0.0699018669780613,0.120491966796142,
0.0158779792746114));
#16930=CARTESIAN_POINT('Ctrl Pts',(-0.0632645460347191,0.123954346655885,
0.0238169689119172));
#16931=CARTESIAN_POINT('Ctrl Pts',(-0.138486976988987,0.0141253725679007,
0.0317559585492228));
#16932=CARTESIAN_POINT('Ctrl Pts',(-0.0869496735326521,-0.108728403071097,
0.0396949481865287));
#16933=CARTESIAN_POINT('Ctrl Pts',(0.0441923146003338,-0.131999388615902,
0.0476339378238343));
#16934=CARTESIAN_POINT('Ctrl Pts',(0.134874939024977,-0.034459980695041,
0.0555729274611401));
#16935=CARTESIAN_POINT('Ctrl Pts',(0.102091080224759,0.094638871230671,
0.0635119170984456));
#16936=CARTESIAN_POINT('Ctrl Pts',(-0.0241513666277066,0.137095110112719,
0.0714509067357516));
#16937=CARTESIAN_POINT('Ctrl Pts',(-0.128284260007319,0.0540539703915629,
0.0793898963730571));
#16938=CARTESIAN_POINT('Ctrl Pts',(-0.114982038412656,-0.0784718756714057,
0.0873288860103631));
#16939=CARTESIAN_POINT('Ctrl Pts',(0.00357853460314598,-0.139161043603659,
0.0952678756476685));
#16940=CARTESIAN_POINT('Ctrl Pts',(0.118863112008681,-0.0724583686054966,
0.103206865284975));
#16941=CARTESIAN_POINT('Ctrl Pts',(0.125336705278751,0.0605752693714656,
0.11114585492228));
#16942=CARTESIAN_POINT('Ctrl Pts',(0.0170731091066207,0.138156245709763,
0.119084844559586));
#16943=CARTESIAN_POINT('Ctrl Pts',(-0.106819734848208,0.0892647286947484,
0.127023834196891));
#16944=CARTESIAN_POINT('Ctrl Pts',(-0.132926439498961,-0.0413425724611633,
0.134962823834197));
#16945=CARTESIAN_POINT('Ctrl Pts',(-0.0373480950846616,-0.134103559412242,
0.142901813471503));
#16946=CARTESIAN_POINT('Ctrl Pts',(0.0924198687735613,-0.104101940294199,
0.150840803108809));
#16947=CARTESIAN_POINT('Ctrl Pts',(0.137583777756591,0.0211978768359354,
0.158779792746114));
#16948=CARTESIAN_POINT('Ctrl Pts',(0.0567991668878991,0.127092487218924,
0.16671878238342));
#16949=CARTESIAN_POINT('Ctrl Pts',(-0.075981188277068,0.116642637502503,
0.174657772020726));
#16950=CARTESIAN_POINT('Ctrl Pts',(-0.139205973057234,-0.000585553717998882,
0.182596761658032));
#16951=CARTESIAN_POINT('Ctrl Pts',(-0.0749972298318695,-0.11727771015962,
0.190535751295337));
#16952=CARTESIAN_POINT('Ctrl Pts',(0.0578663373665801,-0.126610160769685,
0.198474740932643));
#16953=CARTESIAN_POINT('Ctrl Pts',(0.13775723856723,-0.0200396862227523,
0.206413730569949));
#16954=CARTESIAN_POINT('Ctrl Pts',(0.091540828968026,0.104875747581476,
0.214352720207254));
#16955=CARTESIAN_POINT('Ctrl Pts',(-0.0384749358425138,0.133784622116252,
0.22229170984456));
#16956=CARTESIAN_POINT('Ctrl Pts',(-0.133269533752038,0.0402228439430644,
0.230230699481866));
#16957=CARTESIAN_POINT('Ctrl Pts',(-0.106065007067505,-0.0901601911982067,
0.238169689119172));
#16958=CARTESIAN_POINT('Ctrl Pts',(0.0182347644767634,-0.138007750384372,
0.246108678756477));
#16959=CARTESIAN_POINT('Ctrl Pts',(0.125841858853055,-0.0595186723796334,
0.254047668393783));
#16960=CARTESIAN_POINT('Ctrl Pts',(0.118249355954961,0.073455671106145,
0.261986658031089));
#16961=CARTESIAN_POINT('Ctrl Pts',(0.00240767183786234,0.139186381940956,
0.269925647668394));
#16962=CARTESIAN_POINT('Ctrl Pts',(-0.115638070838342,0.0775014991741366,
0.277864637305701));
#16963=CARTESIAN_POINT('Ctrl Pts',(-0.12782508485658,-0.0551306945617612,
0.285803626943006));
#16964=CARTESIAN_POINT('Ctrl Pts',(-0.0229969941138309,-0.137294515779738,
0.293742616580312));
#16965=CARTESIAN_POINT('Ctrl Pts',(0.102883268653204,-0.0937746172089793,
0.301681606217617));
#16966=CARTESIAN_POINT('Ctrl Pts',(0.134580950019115,0.0355895166223291,
0.309620595854923));
#16967=CARTESIAN_POINT('Ctrl Pts',(0.0430789950773988,0.13237388709478,
0.317559585492229));
#16968=CARTESIAN_POINT('Ctrl Pts',(-0.0878588274613298,0.107979036106918,
0.325498575129534));
#16969=CARTESIAN_POINT('Ctrl Pts',(-0.1383679148179,-0.0152632221501787,
0.33343756476684));
#16970=CARTESIAN_POINT('Ctrl Pts',(-0.0622106591311991,-0.12453304658572,
0.341376554404146));
#16971=CARTESIAN_POINT('Ctrl Pts',(0.0708961914151981,-0.119801401679107,
0.349315544041452));
#16972=CARTESIAN_POINT('Ctrl Pts',(0.1391024375543,-0.00539978406154301,
0.357254533678757));
#16973=CARTESIAN_POINT('Ctrl Pts',(0.0799699354250877,0.113944965792994,
0.365193523316063));
#16974=CARTESIAN_POINT('Ctrl Pts',(-0.0523695618881846,0.128980908622551,
0.373132512953369));
#16975=CARTESIAN_POINT('Ctrl Pts',(-0.136768314413298,0.0259436692471295,
0.381071502590675));
#16976=CARTESIAN_POINT('Ctrl Pts',(-0.0959650484377783,-0.100843221288265,
0.38901049222798));
#16977=CARTESIAN_POINT('Ctrl Pts',(0.0326876424682324,-0.135315053971568,
0.396949481865287));
#16978=CARTESIAN_POINT('Ctrl Pts',(0.13141703692502,-0.0459152284901983,
0.404888471502591));
#16979=CARTESIAN_POINT('Ctrl Pts',(0.109843140674695,0.0855168418978295,
0.412827461139898));
#16980=CARTESIAN_POINT('Ctrl Pts',(-0.0122846228212416,0.13866410438033,
0.420766450777203));
#16981=CARTESIAN_POINT('Ctrl Pts',(-0.123166656044517,0.0648738825743514,
0.428705440414509));
#16982=CARTESIAN_POINT('Ctrl Pts',(-0.121298056821252,-0.0683039326309071,
0.436644430051815));
#16983=CARTESIAN_POINT('Ctrl Pts',(-0.00838939967687663,-0.138954178686792,
0.44458341968912));
#16984=CARTESIAN_POINT('Ctrl Pts',(0.11219917790857,-0.0824013973067221,
0.452522409326426));
#16985=CARTESIAN_POINT('Ctrl Pts',(0.13007709763057,0.0495842159710775,
0.460461398963732));
#16986=CARTESIAN_POINT('Ctrl Pts',(0.0288783492374893,0.136178877755608,
0.468400388601037));
#16987=CARTESIAN_POINT('Ctrl Pts',(-0.0987565487199846,0.0981111099028881,
0.476339378238344));
#16988=CARTESIAN_POINT('Ctrl Pts',(-0.135986594552616,-0.0297706550724338,
0.484278367875649));
#16989=CARTESIAN_POINT('Ctrl Pts',(-0.0487302328423073,-0.130399425645183,
0.492217357512954));
#16990=CARTESIAN_POINT('Ctrl Pts',(0.0831353173341669,-0.111656458896056,
0.50015634715026));
#16991=CARTESIAN_POINT('Ctrl Pts',(0.13889618212661,0.00930034365552528,
0.508095336787567));
#16992=CARTESIAN_POINT('Ctrl Pts',(0.0675071113591811,0.12174331898465,
0.516034326424871));
#16993=CARTESIAN_POINT('Ctrl Pts',(-0.0656800932930844,0.122738629397884,
0.523973316062178));
#16994=CARTESIAN_POINT('Ctrl Pts',(-0.138741673886299,0.0113751364249866,
0.531912305699483));
#16995=CARTESIAN_POINT('Ctrl Pts',(-0.0847947606245053,-0.110401514355972,
0.539851295336789));
#16996=CARTESIAN_POINT('Ctrl Pts',(0.0467759446245483,-0.131113145053959,
0.547790284974095));
#16997=CARTESIAN_POINT('Ctrl Pts',(0.135526478334676,-0.031799677225719,
0.555729274611401));
#16998=CARTESIAN_POINT('Ctrl Pts',(0.100211809365564,0.0966242157284558,
0.563668264248707));
#16999=CARTESIAN_POINT('Ctrl Pts',(-0.0268399031138932,0.136595261273209,
0.571607253886012));
#17000=CARTESIAN_POINT('Ctrl Pts',(-0.129321523751272,0.0515227066069736,
0.579546243523318));
#17001=CARTESIAN_POINT('Ctrl Pts',(-0.113418152377209,-0.0807153548762533,
0.587485233160623));
#17002=CARTESIAN_POINT('Ctrl Pts',(0.00631176444456456,-0.139064040754811,
0.595424222797929));
#17003=CARTESIAN_POINT('Ctrl Pts',(0.120263693490807,-0.0701091280034811,
0.603363212435234));
#17004=CARTESIAN_POINT('Ctrl Pts',(0.124122453355413,0.0630258865426945,
0.611302202072541));
#17005=CARTESIAN_POINT('Ctrl Pts',(0.0143556138404206,0.138465021405133,
0.619241191709845));
#17006=CARTESIAN_POINT('Ctrl Pts',(-0.108552806291007,0.0871489187988374,
0.627180181347153));
#17007=CARTESIAN_POINT('Ctrl Pts',(-0.132088571872698,-0.043946046262323,
0.635119170984457));
#17008=CARTESIAN_POINT('Ctrl Pts',(-0.0347063025259737,-0.134811417789573,
0.643058160621763));
#17009=CARTESIAN_POINT('Ctrl Pts',(0.0944472082050275,-0.102266175560326,
0.65099715025907));
#17010=CARTESIAN_POINT('Ctrl Pts',(0.137140772714236,0.0238967416356601,
0.658936139896373));
#17011=CARTESIAN_POINT('Ctrl Pts',(0.054291358674537,0.128183829614862,
0.666875129533682));
#17012=CARTESIAN_POINT('Ctrl Pts',(-0.0782580734018908,0.115127406593233,
0.674814119170985));
#17013=CARTESIAN_POINT('Ctrl Pts',(-0.139167602654929,-0.00332026696803425,
0.682753108808293));
#17014=CARTESIAN_POINT('Ctrl Pts',(-0.0726787294560835,-0.118728463672822,
0.690692098445597));
#17015=CARTESIAN_POINT('Ctrl Pts',(0.0603425395611779,-0.125448888878168,
0.698631088082904));
#17016=CARTESIAN_POINT('Ctrl Pts',(0.138124349154501,-0.0173294538893964,
0.706570077720209));
#17017=CARTESIAN_POINT('Ctrl Pts',(0.0894627833767505,0.106653908470079,
0.714509067357515));
#17018=CARTESIAN_POINT('Ctrl Pts',(-0.0410958292974484,0.133002927094911,
0.72244805699482));
#17019=CARTESIAN_POINT('Ctrl Pts',(-0.134034026730954,0.0375968812502473,
0.730387046632127));
#17020=CARTESIAN_POINT('Ctrl Pts',(-0.104273258644039,-0.0922265326964679,
0.738326036269432));
#17021=CARTESIAN_POINT('Ctrl Pts',(0.0209425314183671,-0.137622876656644,
0.746265025906738));
#17022=CARTESIAN_POINT('Ctrl Pts',(0.126986869252672,-0.0570349089493802,
0.754204015544043));
#17023=CARTESIAN_POINT('Ctrl Pts',(0.11678343126468,0.0757646090434518,
0.762143005181349));
#17024=CARTESIAN_POINT('Ctrl Pts',(-0.000327234354877375,0.139206819944772,
0.770081994818654));
#17025=CARTESIAN_POINT('Ctrl Pts',(-0.117138339349379,0.0752147276530931,
0.778020984455961));
#17026=CARTESIAN_POINT('Ctrl Pts',(-0.126717322684213,-0.0576312930030564,
0.785959974093266));
#17027=CARTESIAN_POINT('Ctrl Pts',(-0.0202952816069424,-0.137719814645367,
0.793898963730571));
#17028=CARTESIAN_POINT('Ctrl Pts',(0.104705698854998,-0.0917352845351548,
0.801837953367879));
#17029=CARTESIAN_POINT('Ctrl Pts',(0.133855787965376,0.0382266115373486,
0.809776943005182));
#17030=CARTESIAN_POINT('Ctrl Pts',(0.0404700769297216,0.133194664588195,
0.81771593264249));
#17031=CARTESIAN_POINT('Ctrl Pts',(-0.0899632159395838,0.106232130635072,
0.825654922279794));
#17032=CARTESIAN_POINT('Ctrl Pts',(-0.13804135019805,-0.0179786383510676,
0.833593911917101));
#17033=CARTESIAN_POINT('Ctrl Pts',(-0.059752088941783,-0.125731196083361,
0.841532901554406));
#17034=CARTESIAN_POINT('Ctrl Pts',(0.0732361146625898,-0.118385460722959,
0.849471891191712));
#17035=CARTESIAN_POINT('Ctrl Pts',(0.139181674492094,-0.00266594955618734,
0.857410880829018));
#17036=CARTESIAN_POINT('Ctrl Pts',(0.077715950067195,0.115494055719818,
0.865349870466323));
#17037=CARTESIAN_POINT('Ctrl Pts',(-0.0548934004223171,0.127927168308903,
0.87328886010363));
#17038=CARTESIAN_POINT('Ctrl Pts',(-0.137251604915624,0.0232517257326144,
0.881227849740934));
#17039=CARTESIAN_POINT('Ctrl Pts',(-0.0939653715754795,-0.102709078207047,
0.889166839378241));
#17040=CARTESIAN_POINT('Ctrl Pts',(0.0353397195745277,-0.134646760160997,
0.897105829015547));
#17041=CARTESIAN_POINT('Ctrl Pts',(0.132293719443212,-0.0433245611326863,
0.905044818652852));
#17042=CARTESIAN_POINT('Ctrl Pts',(0.108141885842356,0.0876583043865096,
0.912983808290157));
#17043=CARTESIAN_POINT('Ctrl Pts',(-0.0150064327997127,0.138395999855801,
0.920922797927463));
#17044=CARTESIAN_POINT('Ctrl Pts',(-0.124417390671652,0.0624416423544169,
0.928861787564769));
#17045=CARTESIAN_POINT('Ctrl Pts',(-0.119932754264349,-0.0706737593172073,
0.936800777202075));
#17046=CARTESIAN_POINT('Ctrl Pts',(-0.00565790085648466,-0.139092177922979,
0.944739766839381));
#17047=CARTESIAN_POINT('Ctrl Pts',(0.113796373024222,-0.0801812402497705,
0.952678756476687));
#17048=CARTESIAN_POINT('Ctrl Pts',(0.129077866376032,0.0521301276928276,
0.960617746113992));
#17049=CARTESIAN_POINT('Ctrl Pts',(0.026197419344502,0.13671993644362,0.968556735751298));
#17050=CARTESIAN_POINT('Ctrl Pts',(-0.100664969670515,0.0961520134094621,
0.976495725388603));
#17051=CARTESIAN_POINT('Ctrl Pts',(-0.13537547797311,-0.0324364881732178,
0.98443471502591));
#17052=CARTESIAN_POINT('Ctrl Pts',(-0.0461590140787468,-0.131331607851033,
0.992373704663214));
#17053=CARTESIAN_POINT('Ctrl Pts',(0.0853128637208732,-0.110001641284132,
1.00031269430052));
#17054=CARTESIAN_POINT('Ctrl Pts',(0.138686661656432,0.0120272889735618,
1.00825168393783));
#17055=CARTESIAN_POINT('Ctrl Pts',(0.0651023256631918,0.123046060459907,
1.01619067357513));
#17056=CARTESIAN_POINT('Ctrl Pts',(-0.0680787277209358,0.121424596492465,
1.02412966321244));
#17057=CARTESIAN_POINT('Ctrl Pts',(-0.138938371616466,0.00864723620724691,
1.03206865284975));
#17058=CARTESIAN_POINT('Ctrl Pts',(-0.0826094583655966,-0.112046076191904,
1.04000764248705));
#17059=CARTESIAN_POINT('Ctrl Pts',(0.0493427524230464,-0.130168884856471,
1.04794663212436));
#17060=CARTESIAN_POINT('Ctrl Pts',(0.136125055048066,-0.0291310004912345,
1.05588562176166));
#17061=CARTESIAN_POINT('Ctrl Pts',(0.0982941990358779,0.0985743183458784,
1.06382461139897));
#17062=CARTESIAN_POINT('Ctrl Pts',(-0.0295182596522469,0.136041604476578,
1.07176360103627));
#17063=CARTESIAN_POINT('Ctrl Pts',(-0.130308774647192,0.0489721252490281,
1.07970259067358));
#17064=CARTESIAN_POINT('Ctrl Pts',(-0.111810537096203,-0.0829279783650712,
1.08764158031088));
#17065=CARTESIAN_POINT('Ctrl Pts',(0.00904258428980543,-0.13891320121148,
1.09558056994819));
#17066=CARTESIAN_POINT('Ctrl Pts',(0.121617839487272,-0.067732908692211,
1.1035195595855));
#17067=CARTESIAN_POINT('Ctrl Pts',(0.122860297649024,0.0654522196953821,
1.1114585492228));
#17068=CARTESIAN_POINT('Ctrl Pts',(0.0116325734791967,0.138720326685422,
1.11939753886011));
#17069=CARTESIAN_POINT('Ctrl Pts',(-0.110243974478508,0.0849994817198388,
1.12733652849741));
#17070=CARTESIAN_POINT('Ctrl Pts',(-0.131199719314147,-0.0465325633653302,
1.13527551813472));
#17071=CARTESIAN_POINT('Ctrl Pts',(-0.0320511128216771,-0.13546723577438,
1.14321450777202));
#17072=CARTESIAN_POINT('Ctrl Pts',(0.0964380908528195,-0.100390938007982,
1.15115349740933));
#17073=CARTESIAN_POINT('Ctrl Pts',(0.136644831685568,0.0265863832644056,
1.15909248704664));
#17074=CARTESIAN_POINT('Ctrl Pts',(0.0517625939920979,0.129225692742072,
1.16703147668394));
#17075=CARTESIAN_POINT('Ctrl Pts',(-0.0805047509788913,0.113567736929491,
1.17497046632125));
#17076=CARTESIAN_POINT('Ctrl Pts',(-0.139075513779617,-0.00605369873671642,
1.18290945595855));
#17077=CARTESIAN_POINT('Ctrl Pts',(-0.0703321751825429,-0.12013338809653,
1.19084844559586));
#17078=CARTESIAN_POINT('Ctrl Pts',(0.0627954496153871,-0.124239193932754,
1.19878743523316));
#17079=CARTESIAN_POINT('Ctrl Pts',(0.138438143943654,-0.0146125323915816,
1.20672642487047));
#17080=CARTESIAN_POINT('Ctrl Pts',(0.0873502052771435,0.108390901091839,
1.21466541450777));
#17081=CARTESIAN_POINT('Ctrl Pts',(-0.043700859820065,0.132169893139269,
1.22260440414508));
#17082=CARTESIAN_POINT('Ctrl Pts',(-0.134746782767514,0.0349564062120582,
1.23054339378239));
#17083=CARTESIAN_POINT('Ctrl Pts',(-0.102441260891455,-0.0942572748833364,
1.23848238341969));
#17084=CARTESIAN_POINT('Ctrl Pts',(0.0236422145726536,-0.137184880695923,
1.246421373057));
#17085=CARTESIAN_POINT('Ctrl Pts',(0.128082862902196,-0.0545291301253663,
1.2543603626943));
#17086=CARTESIAN_POINT('Ctrl Pts',(0.115272428336817,0.0780443019497631,
1.26229935233161));
#17087=CARTESIAN_POINT('Ctrl Pts',(-0.00306201423577413,0.139173524314926,
1.27023834196891));
#17088=CARTESIAN_POINT('Ctrl Pts',(-0.118593392628464,0.0728989233548558,
1.27817733160622));
#17089=CARTESIAN_POINT('Ctrl Pts',(-0.125560647806918,-0.06010964584811,
1.28611632124353));
#17090=CARTESIAN_POINT('Ctrl Pts',(-0.0175857351491984,-0.138091953858251,
1.29405531088083));
#17091=CARTESIAN_POINT('Ctrl Pts',(0.106487712804436,-0.089660542174548,
1.30199430051814));
#17092=CARTESIAN_POINT('Ctrl Pts',(0.133078957772855,0.0408489510387311,
1.30993329015544));
#17093=CARTESIAN_POINT('Ctrl Pts',(0.0378455373822902,0.133964029124136,
1.31787227979275));
#17094=CARTESIAN_POINT('Ctrl Pts',(-0.0920328787300654,0.104444219726284,
1.32581126943006));
#17095=CARTESIAN_POINT('Ctrl Pts',(-0.137661501842601,-0.0206871148492911,
1.33375025906736));
#17096=CARTESIAN_POINT('Ctrl Pts',(-0.0572704544775333,-0.126880813469472,
1.34168924870467));
#17097=CARTESIAN_POINT('Ctrl Pts',(0.0755477687720905,-0.116923823242002,
1.34962823834197));
#17098=CARTESIAN_POINT('Ctrl Pts',(0.13920718769651,6.89141801743488E-5,
1.35756722797928));
#17099=CARTESIAN_POINT('Ctrl Pts',(0.0754319660950179,0.116998564767658,
1.36550621761658));
#17100=CARTESIAN_POINT('Ctrl Pts',(-0.0573960494825499,0.126824048933643,
1.37344520725389));
#17101=CARTESIAN_POINT('Ctrl Pts',(-0.13768191782304,0.0205508058651932,
1.38138419689119));
#17102=CARTESIAN_POINT('Ctrl Pts',(-0.0919294216917856,-0.104535287252199,
1.3893231865285));
#17103=CARTESIAN_POINT('Ctrl Pts',(0.0379781508110965,-0.133926497290667,
1.39726217616581));
#17104=CARTESIAN_POINT('Ctrl Pts',(0.133119345865688,-0.0407171622080862,
1.40520116580311));
#17105=CARTESIAN_POINT('Ctrl Pts',(0.106398871137127,0.0897659150453452,
1.41314015544042));
#17106=CARTESIAN_POINT('Ctrl Pts',(-0.0177224175491345,0.138074504763813,
1.42107914507772));
#17107=CARTESIAN_POINT('Ctrl Pts',(-0.125620162573399,0.0599852426217579,
1.42901813471503));
#17108=CARTESIAN_POINT('Ctrl Pts',(-0.118521039729242,-0.0730161975746823,
1.43695712435233));
#17109=CARTESIAN_POINT('Ctrl Pts',(-0.00292444232197888,-0.139176693688359,
1.44489611398964));
#17110=CARTESIAN_POINT('Ctrl Pts',(0.115350068603298,-0.0779297424218237,
1.45283510362695));
#17111=CARTESIAN_POINT('Ctrl Pts',(0.128028003046829,0.0546551750765237,
1.46077409326425));
#17112=CARTESIAN_POINT('Ctrl Pts',(0.0235079116789307,0.137209630484779,
1.46871308290156));
#17113=CARTESIAN_POINT('Ctrl Pts',(-0.102537447198224,0.0941531272373115,
1.47665207253886));
#17114=CARTESIAN_POINT('Ctrl Pts',(-0.134706575776555,-0.0350847218495708,
1.48459106217617));
#17115=CARTESIAN_POINT('Ctrl Pts',(-0.0435804807853106,-0.132222740314769,
1.49253005181348));
#17116=CARTESIAN_POINT('Ctrl Pts',(0.0874774386997331,-0.108286040948335,
1.50046904145078));
#17117=CARTESIAN_POINT('Ctrl Pts',(0.138385550162814,0.0147146982980264,
1.50840803108809));
#17118=CARTESIAN_POINT('Ctrl Pts',(0.0627460642121078,0.124368470664037,
1.51634702072539));
#17119=CARTESIAN_POINT('Ctrl Pts',(-0.0706026869052757,0.119928391791904,
1.5242860103627));
#17120=CARTESIAN_POINT('Ctrl Pts',(-0.116004137797729,0.0441355889673283,
1.5295786701209));
#17121=CARTESIAN_POINT('Ctrl Pts',(-0.117668597464313,0.00500517689812487,
1.532225));
#17122=CARTESIAN_POINT('',(0.0684664424539461,-0.0958295198918396,0.));
#17123=CARTESIAN_POINT('Ctrl Pts',(0.0684664424539414,-0.095829519891843,
-1.38777878078145E-17));
#17124=CARTESIAN_POINT('Ctrl Pts',(0.100334321247169,-0.0730611673843044,
0.00264632987910189));
#17125=CARTESIAN_POINT('Ctrl Pts',(0.139021564822767,0.00636891437108143,
0.00793898963730573));
#17126=CARTESIAN_POINT('Ctrl Pts',(0.0699018669780613,0.120491966796142,
0.0158779792746114));
#17127=CARTESIAN_POINT('Ctrl Pts',(-0.0632645460347191,0.123954346655885,
0.0238169689119172));
#17128=CARTESIAN_POINT('Ctrl Pts',(-0.11596266760442,0.0470121293552651,
0.0293787386625077));
#17129=CARTESIAN_POINT('Ctrl Pts',(-0.117944740497024,0.00404481602818191,
0.0322941785339964));
#17130=CARTESIAN_POINT('Ctrl Pts',(-0.117917485785546,7.60014832213644E-5,
0.0325632885263832));
#17131=CARTESIAN_POINT('Ctrl Pts',(0.0635546915223951,0.132092229195826,
-2.16840434497101E-19));
#17132=CARTESIAN_POINT('Ctrl Pts',(0.0668114782730532,0.13015255741457,
-1.00603861447787E-18));
#17133=CARTESIAN_POINT('Ctrl Pts',(0.0699821360194518,0.12808121947321,
-2.9262196004085E-17));
#17134=CARTESIAN_POINT('Ctrl Pts',(0.0730575207853233,0.125877721325919,
-2.71050543121376E-17));
#17135=CARTESIAN_POINT('Ctrl Pts',(0.0789281193465506,0.121671466161783,
-2.36378102375718E-17));
#17136=CARTESIAN_POINT('Ctrl Pts',(0.0844522091809674,0.11698398814956,
1.43782932504085E-18));
#17137=CARTESIAN_POINT('Ctrl Pts',(0.0895990070394484,0.111875963994554,
9.97465998686664E-18));
#17138=CARTESIAN_POINT('Ctrl Pts',(0.0928865546640729,0.108613183302742,
1.54276111490851E-17));
#17139=CARTESIAN_POINT('Ctrl Pts',(0.0960206821069302,0.105176950779614,
-2.53636710091701E-17));
#17140=CARTESIAN_POINT('Ctrl Pts',(0.098978417360439,0.101599719103904,
-1.56125112837913E-17));
#17141=CARTESIAN_POINT('Ctrl Pts',(0.103148772110026,0.0965558852815647,
-1.86354736740503E-18));
#17142=CARTESIAN_POINT('Ctrl Pts',(0.106976174326278,0.0912251680483688,
1.1337629845105E-17));
#17143=CARTESIAN_POINT('Ctrl Pts',(0.110435561611279,0.0856523061447448,
2.03830008427275E-17));
#17144=CARTESIAN_POINT('Ctrl Pts',(0.112407683932559,0.0824753373788608,
2.55395723911076E-17));
#17145=CARTESIAN_POINT('Ctrl Pts',(0.114261188142284,0.0792174064057451,
2.29308760465575E-17));
#17146=CARTESIAN_POINT('Ctrl Pts',(0.115986535786665,0.0758936579718971,
2.08166817117217E-17));
#17147=CARTESIAN_POINT('Ctrl Pts',(0.120573220307724,0.0670577659456877,
1.51962825639422E-17));
#17148=CARTESIAN_POINT('Ctrl Pts',(0.124235263225439,0.0578042025119142,
2.52358375750583E-18));
#17149=CARTESIAN_POINT('Ctrl Pts',(0.126883306113679,0.0482911783993335,
1.30104260698261E-17));
#17150=CARTESIAN_POINT('Ctrl Pts',(0.128478610866444,0.0425600882242624,
1.93281898253259E-17));
#17151=CARTESIAN_POINT('Ctrl Pts',(0.129704960854084,0.0367345196138549,
-5.78096029915021E-19));
#17152=CARTESIAN_POINT('Ctrl Pts',(0.130533291754837,0.0308494671050701,
0.));
#17153=CARTESIAN_POINT('Ctrl Pts',(0.131003715791213,0.0275072397983871,
3.2831114661813E-19));
#17154=CARTESIAN_POINT('Ctrl Pts',(0.131345346899704,0.0241444941465381,
-1.7128612844445E-18));
#17155=CARTESIAN_POINT('Ctrl Pts',(0.131551728167405,0.0207857616715298,
2.60208521396521E-18));
#17156=CARTESIAN_POINT('Ctrl Pts',(0.131851321606701,0.0159100565018035,
8.86587880453295E-18));
#17157=CARTESIAN_POINT('Ctrl Pts',(0.131867617692795,0.0110341713389591,
-1.68111772803455E-17));
#17158=CARTESIAN_POINT('Ctrl Pts',(0.131586936334964,0.0061777758930637,
-6.93889390390723E-18));
#17159=CARTESIAN_POINT('Ctrl Pts',(0.131099036368572,-0.00226395031615145,
9.98510028643051E-18));
#17160=CARTESIAN_POINT('Ctrl Pts',(0.129715139118287,-0.0106479390144509,
1.03491660509995E-17));
#17161=CARTESIAN_POINT('Ctrl Pts',(0.127493709984164,-0.018859987399606,
1.04083408558608E-17));
#17162=CARTESIAN_POINT('Ctrl Pts',(0.126553994220251,-0.0223338732882013,
1.04333731632617E-17));
#17163=CARTESIAN_POINT('Ctrl Pts',(0.125463061762623,-0.0257782540966497,
1.75224609115742E-17));
#17164=CARTESIAN_POINT('Ctrl Pts',(0.124232565886791,-0.0291638780753137,
1.73472347597681E-17));
#17165=CARTESIAN_POINT('Ctrl Pts',(0.12170396813588,-0.0361211392462112,
1.69871551674183E-17));
#17166=CARTESIAN_POINT('Ctrl Pts',(0.118582485980247,-0.0428512226170345,
-6.45748389186585E-19));
#17167=CARTESIAN_POINT('Ctrl Pts',(0.114911168983798,-0.0492778939609075,
3.46944695195361E-18));
#17168=CARTESIAN_POINT('Ctrl Pts',(0.112347970921096,-0.0537647937721124,
6.34254691478841E-18));
#17169=CARTESIAN_POINT('Ctrl Pts',(0.109516356061708,-0.0581036184196785,
-1.05628593522785E-17));
#17170=CARTESIAN_POINT('Ctrl Pts',(0.106427098863261,-0.0622637901458048,
-1.21430643318376E-17));
#17171=CARTESIAN_POINT('Ctrl Pts',(0.104287070791936,-0.0651456752410043,
-1.32377232732828E-17));
#17172=CARTESIAN_POINT('Ctrl Pts',(0.102021590876101,-0.067943056099314,
-1.03088264066386E-17));
#17173=CARTESIAN_POINT('Ctrl Pts',(0.0996491962474235,-0.0706287444932102,
-1.04083408558608E-17));
#17174=CARTESIAN_POINT('Ctrl Pts',(0.0938611946766418,-0.0771810981592459,
-1.06511292104842E-17));
#17175=CARTESIAN_POINT('Ctrl Pts',(0.0874218747326319,-0.0830961188460978,
9.460259835177E-18));
#17176=CARTESIAN_POINT('Ctrl Pts',(0.0803902102994179,-0.0882260767030795,
2.94902990916057E-17));
#17177=CARTESIAN_POINT('Ctrl Pts',(0.0765868618375105,-0.091000813397402,
4.03243227742548E-17));
#17178=CARTESIAN_POINT('Ctrl Pts',(0.0726097989303321,-0.0935451549285004,
-2.49510848448888E-18));
#17179=CARTESIAN_POINT('Ctrl Pts',(0.0684664424539416,-0.0958295198918429,
0.));
#17180=CARTESIAN_POINT('Ctrl Pts',(-0.00156962371674571,0.146072546381438,
1.50365));
#17181=CARTESIAN_POINT('Ctrl Pts',(0.0218361081466035,0.146362061217761,
1.50238307892777));
#17182=CARTESIAN_POINT('Ctrl Pts',(0.0452966847593804,0.141345883428421,
1.50111615785553));
#17183=CARTESIAN_POINT('Ctrl Pts',(0.0660179268768178,0.130913916311315,
1.4998492367833));
#17184=CARTESIAN_POINT('Ctrl Pts',(0.109300214423576,0.109123745727819,
1.4972029069042));
#17185=CARTESIAN_POINT('Ctrl Pts',(0.140630685714559,0.0637042888941242,
1.49455657702509));
#17186=CARTESIAN_POINT('Ctrl Pts',(0.145752650840527,0.0155206226173656,
1.49191024714599));
#17187=CARTESIAN_POINT('Ctrl Pts',(0.150874615966495,-0.0326630436593903,
1.48926391726689));
#17188=CARTESIAN_POINT('Ctrl Pts',(0.129788074927449,-0.0836109193792113,
1.48661758738779));
#17189=CARTESIAN_POINT('Ctrl Pts',(0.0921021927661857,-0.114042242015571,
1.48397125750869));
#17190=CARTESIAN_POINT('Ctrl Pts',(0.0544163106049216,-0.144473564651931,
1.48132492762959));
#17191=CARTESIAN_POINT('Ctrl Pts',(0.000131087321441313,-0.154388334204831,
1.47867859775048));
#17192=CARTESIAN_POINT('Ctrl Pts',(-0.0458840977328367,-0.139228052523514,
1.47603226787138));
#17193=CARTESIAN_POINT('Ctrl Pts',(-0.0918992827871148,-0.124067770842196,
1.47338593799228));
#17194=CARTESIAN_POINT('Ctrl Pts',(-0.129644429612189,-0.0838324379266627,
1.47073960811318));
#17195=CARTESIAN_POINT('Ctrl Pts',(-0.141854649713415,-0.0369491035797489,
1.46809327823408));
#17196=CARTESIAN_POINT('Ctrl Pts',(-0.14497337938942,-0.0249741805295802,
1.46741735368415));
#17197=CARTESIAN_POINT('Ctrl Pts',(-0.146426231435716,-0.0125655473306973,
1.46674142913422));
#17198=CARTESIAN_POINT('Ctrl Pts',(-0.14631473222987,-0.000131398079681141,
1.46606550458429));
#17199=CARTESIAN_POINT('Origin',(0.,0.,-0.0924367114736175));
#17200=CARTESIAN_POINT('',(-0.0684664424539507,-0.0958295198918364,0.));
#17201=CARTESIAN_POINT('Ctrl Pts',(-0.0686146973663072,-0.0959584553529141,
8.16675286424706E-17));
#17202=CARTESIAN_POINT('Ctrl Pts',(-0.0391968190522335,-0.116741470120209,
0.00244290680874874));
#17203=CARTESIAN_POINT('Ctrl Pts',(0.0436301113039178,-0.130476273073809,
0.0075332029917574));
#17204=CARTESIAN_POINT('Ctrl Pts',(0.134092250525203,-0.0374520209666004,
0.0152708885490261));
#17205=CARTESIAN_POINT('Ctrl Pts',(0.104134301645602,0.0924305194826295,
0.023213056671806));
#17206=CARTESIAN_POINT('Ctrl Pts',(-0.0212379681243542,0.137589894578696,
0.0311552247945861));
#17207=CARTESIAN_POINT('Ctrl Pts',(-0.106685947947232,0.0723488109778776,
0.0375631097285225));
#17208=CARTESIAN_POINT('Ctrl Pts',(-0.117663533972591,0.0165813593984342,
0.041323605288199));
#17209=CARTESIAN_POINT('Ctrl Pts',(-0.117600989619072,5.04992496179954E-5,
0.0424367114736154));
#17210=CARTESIAN_POINT('Origin',(0.,0.,0.));
#17211=CARTESIAN_POINT('Ctrl Pts',(-0.0510216505388318,0.106149619882943,
-0.0164977839420939));
#17212=CARTESIAN_POINT('Ctrl Pts',(-0.0863355867949722,0.0891756983861136,
-0.0138503945678339));
#17213=CARTESIAN_POINT('Ctrl Pts',(-0.13808023131828,0.0175094743621551,
-0.00855561581931395));
#17214=CARTESIAN_POINT('Ctrl Pts',(-0.0894531427980795,-0.106808298616542,
-0.000613447696533924));
#17215=CARTESIAN_POINT('Ctrl Pts',(0.0412394829729132,-0.132934609947913,
0.00732872042624606));
#17216=CARTESIAN_POINT('Ctrl Pts',(0.134092250525203,-0.0374520209666004,
0.0152708885490261));
#17217=CARTESIAN_POINT('Ctrl Pts',(0.104134301645602,0.0924305194826295,
0.023213056671806));
#17218=CARTESIAN_POINT('Ctrl Pts',(-0.0212379681243542,0.137589894578696,
0.0311552247945861));
#17219=CARTESIAN_POINT('Ctrl Pts',(-0.127145335141994,0.0567276974868182,
0.039097392917366));
#17220=CARTESIAN_POINT('Ctrl Pts',(-0.116579117211717,-0.0761160149501382,
0.0470395610401461));
#17221=CARTESIAN_POINT('Ctrl Pts',(0.000787973702835166,-0.139222729671589,
0.054981729162926));
#17222=CARTESIAN_POINT('Ctrl Pts',(0.117431922513572,-0.0747907597173192,
0.0629238972857061));
#17223=CARTESIAN_POINT('Ctrl Pts',(0.126496838785129,0.0581591461343325,
0.070866065408486));
#17224=CARTESIAN_POINT('Ctrl Pts',(0.0196773008918215,0.137828289815661,
0.0788082335312661));
#17225=CARTESIAN_POINT('Ctrl Pts',(-0.105168479521776,0.0912330920368172,
0.0867504016540459));
#17226=CARTESIAN_POINT('Ctrl Pts',(-0.133669226619255,-0.0389412707994331,
0.0946925697768262));
#17227=CARTESIAN_POINT('Ctrl Pts',(-0.0397151780004399,-0.133441281507892,
0.102634737899606));
#17228=CARTESIAN_POINT('Ctrl Pts',(0.0906220264938673,-0.105695447092796,
0.110576906022386));
#17229=CARTESIAN_POINT('Ctrl Pts',(0.137940159127448,0.0188783162799928,
0.118519074145166));
#17230=CARTESIAN_POINT('Ctrl Pts',(0.0588909273047484,0.126157580947307,
0.126461242267946));
#17231=CARTESIAN_POINT('Ctrl Pts',(-0.074108440039672,0.117863552156501,
0.134403410390726));
#17232=CARTESIAN_POINT('Ctrl Pts',(-0.139216864956951,0.00159439502933392,
0.142345578513506));
#17233=CARTESIAN_POINT('Ctrl Pts',(-0.0767883381764272,-0.116135388594389,
0.150287746636286));
#17234=CARTESIAN_POINT('Ctrl Pts',(0.0559861945572589,-0.127473226882309,
0.158229914759066));
#17235=CARTESIAN_POINT('Ctrl Pts',(0.137471621702818,-0.0220324926503626,
0.166172082881846));
#17236=CARTESIAN_POINT('Ctrl Pts',(0.0930189202108026,0.103592267873211,
0.174114251004626));
#17237=CARTESIAN_POINT('Ctrl Pts',(-0.0366486683060043,0.134315868829211,
0.182056419127406));
#17238=CARTESIAN_POINT('Ctrl Pts',(-0.132742311638566,0.0419923350165386,
0.189998587250186));
#17239=CARTESIAN_POINT('Ctrl Pts',(-0.107230360350792,-0.0888004916405464,
0.197940755372966));
#17240=CARTESIAN_POINT('Ctrl Pts',(0.0165156171993534,-0.138242945169174,
0.205882923495746));
#17241=CARTESIAN_POINT('Ctrl Pts',(0.125131592687617,-0.061040658666823,
0.213825091618526));
#17242=CARTESIAN_POINT('Ctrl Pts',(0.119114174013628,0.0720811421096423,
0.221767259741306));
#17243=CARTESIAN_POINT('Ctrl Pts',(0.0039759348809324,0.139169211541763,
0.229709427864086));
#17244=CARTESIAN_POINT('Ctrl Pts',(-0.114804669066963,0.0787639858025777,
0.237651595986866));
#17245=CARTESIAN_POINT('Ctrl Pts',(-0.128412401817242,-0.0537971426620367,
0.245593764109646));
#17246=CARTESIAN_POINT('Ctrl Pts',(-0.024381182195918,-0.137074561658528,
0.253535932232426));
#17247=CARTESIAN_POINT('Ctrl Pts',(0.101985705091022,-0.094777599970642,
0.261478100355206));
#17248=CARTESIAN_POINT('Ctrl Pts',(0.134923209124943,0.0343453801629359,
0.269420268477986));
#17249=CARTESIAN_POINT('Ctrl Pts',(0.0442571924125319,0.132004463632409,
0.277362436600766));
#17250=CARTESIAN_POINT('Ctrl Pts',(-0.0869529592639067,0.108733897080731,
0.285304604723546));
#17251=CARTESIAN_POINT('Ctrl Pts',(-0.138505267237684,-0.0141480898545381,
0.293246772846326));
#17252=CARTESIAN_POINT('Ctrl Pts',(-0.0631725212350128,-0.124068972994571,
0.301188940969106));
#17253=CARTESIAN_POINT('Ctrl Pts',(0.0700327441786229,-0.12032993078169,
0.309131109091886));
#17254=CARTESIAN_POINT('Ctrl Pts',(0.139080821187468,-0.00635631000930847,
0.317073277214666));
#17255=CARTESIAN_POINT('Ctrl Pts',(0.0807165776729536,0.11344034374014,
0.325015445337446));
#17256=CARTESIAN_POINT('Ctrl Pts',(-0.0515923433190751,0.129313988454311,
0.332957613460226));
#17257=CARTESIAN_POINT('Ctrl Pts',(-0.136637377548019,0.026722734813544,
0.340899781583006));
#17258=CARTESIAN_POINT('Ctrl Pts',(-0.0965085366518414,-0.100349289247285,
0.348841949705786));
#17259=CARTESIAN_POINT('Ctrl Pts',(0.0320320385160992,-0.135491055083419,
0.356784117828566));
#17260=CARTESIAN_POINT('Ctrl Pts',(0.131227975626944,-0.0465090949381858,
0.364726285951346));
#17261=CARTESIAN_POINT('Ctrl Pts',(0.110205605501345,0.0850799742312894,
0.372668454074126));
#17262=CARTESIAN_POINT('Ctrl Pts',(-0.0117764211155082,0.138727046407055,
0.380610622196906));
#17263=CARTESIAN_POINT('Ctrl Pts',(-0.122970036152848,0.065285892102983,
0.388552790319686));
#17264=CARTESIAN_POINT('Ctrl Pts',(-0.121510464882371,-0.0679638464419502,
0.396494958442466));
#17265=CARTESIAN_POINT('Ctrl Pts',(-0.00873482453528946,-0.138951719454826,
0.404437126565246));
#17266=CARTESIAN_POINT('Ctrl Pts',(0.112042812448737,-0.0826455423945668,
0.412379294688026));
#17267=CARTESIAN_POINT('Ctrl Pts',(0.130177722634257,0.049372441998279,
0.420321462810806));
#17268=CARTESIAN_POINT('Ctrl Pts',(0.0290564652212241,0.136160197297018,
0.428263630933586));
#17269=CARTESIAN_POINT('Ctrl Pts',(-0.098683499418539,0.098211223603141,
0.436205799056366));
#17270=CARTESIAN_POINT('Ctrl Pts',(-0.136019240449831,-0.0297093205335648,
0.444147967179146));
#17271=CARTESIAN_POINT('Ctrl Pts',(-0.0487473834415776,-0.130413074907061,
0.452090135301926));
#17272=CARTESIAN_POINT('Ctrl Pts',(0.0831820848081396,-0.111645054821459,
0.460032303424706));
#17273=CARTESIAN_POINT('Ctrl Pts',(0.138908217753341,0.00940130521287039,
0.467974471547486));
#17274=CARTESIAN_POINT('Ctrl Pts',(0.0673801526530663,0.121835103839429,
0.475916639670265));
#17275=CARTESIAN_POINT('Ctrl Pts',(-0.0658750545035054,0.12265543075329,
0.483858807793047));
#17276=CARTESIAN_POINT('Ctrl Pts',(-0.138781944133385,0.0111107822259715,
0.491800975915825));
#17277=CARTESIAN_POINT('Ctrl Pts',(-0.084550315326251,-0.110612484274364,
0.499743144038607));
#17278=CARTESIAN_POINT('Ctrl Pts',(0.0471380885036503,-0.131003351527116,
0.507685312161385));
#17279=CARTESIAN_POINT('Ctrl Pts',(0.135643160584381,-0.031381690295376,
0.515627480284167));
#17280=CARTESIAN_POINT('Ctrl Pts',(0.0998851624184703,0.0969888232104648,
0.523569648406945));
#17281=CARTESIAN_POINT('Ctrl Pts',(-0.0273779061153799,0.136507610615132,
0.531511816529727));
#17282=CARTESIAN_POINT('Ctrl Pts',(-0.129560000008381,0.0509714027366644,
0.539453984652505));
#17283=CARTESIAN_POINT('Ctrl Pts',(-0.113051823689188,-0.0812598465397498,
0.547396152775286));
#17284=CARTESIAN_POINT('Ctrl Pts',(0.00702343738442799,-0.139048728244533,
0.555338320898066));
#17285=CARTESIAN_POINT('Ctrl Pts',(0.12066450826877,-0.0694546898587181,
0.563280489020846));
#17286=CARTESIAN_POINT('Ctrl Pts',(0.123764493242992,0.063766979789076,
0.571222657143626));
#17287=CARTESIAN_POINT('Ctrl Pts',(0.0134834875971477,0.13857154491934,
0.579164825266405));
#17288=CARTESIAN_POINT('Ctrl Pts',(-0.109149777898995,0.0864303389077871,
0.587106993389186));
#17289=CARTESIAN_POINT('Ctrl Pts',(-0.131790633456927,-0.0448899368693808,
0.595049161511966));
#17290=CARTESIAN_POINT('Ctrl Pts',(-0.0336977294021144,-0.135086418755761,
0.602991329634746));
#17291=CARTESIAN_POINT('Ctrl Pts',(0.0952657566843092,-0.101529863106778,
0.610933497757526));
#17292=CARTESIAN_POINT('Ctrl Pts',(0.136956022624868,0.025038477707157,
0.618875665880307));
#17293=CARTESIAN_POINT('Ctrl Pts',(0.0531805018142573,0.128669000640787,
0.626817834003085));
#17294=CARTESIAN_POINT('Ctrl Pts',(-0.0793138220987445,0.114425500318782,
0.634760002125867));
#17295=CARTESIAN_POINT('Ctrl Pts',(-0.139148536750765,-0.00464351367351466,
0.642702170248646));
#17296=CARTESIAN_POINT('Ctrl Pts',(-0.0715088964667609,-0.119458592094588,
0.650644338371427));
#17297=CARTESIAN_POINT('Ctrl Pts',(0.0616402393688536,-0.124837327709565,
0.658586506494205));
#17298=CARTESIAN_POINT('Ctrl Pts',(0.138320583400205,-0.0158522461166236,
0.666528674616987));
#17299=CARTESIAN_POINT('Ctrl Pts',(0.0882850628235238,0.107655121482266,
0.674470842739765));
#17300=CARTESIAN_POINT('Ctrl Pts',(-0.0426286451686149,0.132539337972556,
0.682413010862546));
#17301=CARTESIAN_POINT('Ctrl Pts',(-0.13449013477919,0.0360039045964495,
0.690355178985326));
#17302=CARTESIAN_POINT('Ctrl Pts',(-0.103144844235522,-0.0935148042116587,
0.698297347108106));
#17303=CARTESIAN_POINT('Ctrl Pts',(0.022691720100341,-0.137364345221032,
0.706239515230886));
#17304=CARTESIAN_POINT('Ctrl Pts',(0.127740337615313,-0.0553740340325759,
0.714181683353665));
#17305=CARTESIAN_POINT('Ctrl Pts',(0.115765682611161,0.077344581120379,
0.722123851476446));
#17306=CARTESIAN_POINT('Ctrl Pts',(-0.00226223072526165,0.139207614056346,
0.730066019599226));
#17307=CARTESIAN_POINT('Ctrl Pts',(-0.118217708309552,0.0735421711751344,
0.738008187722006));
#17308=CARTESIAN_POINT('Ctrl Pts',(-0.125873620115675,-0.059495455776806,
0.745950355844786));
#17309=CARTESIAN_POINT('Ctrl Pts',(-0.0182163644075178,-0.138029133036789,
0.753892523967566));
#17310=CARTESIAN_POINT('Ctrl Pts',(0.106128952536144,-0.0901139441634624,
0.761834692090347));
#17311=CARTESIAN_POINT('Ctrl Pts',(0.133249245915149,0.0403548753208232,
0.769776860213125));
#17312=CARTESIAN_POINT('Ctrl Pts',(0.0382995408207276,0.133854483197375,
0.777719028335907));
#17313=CARTESIAN_POINT('Ctrl Pts',(-0.0917364783268051,0.104729633071593,
0.785661196458685));
#17314=CARTESIAN_POINT('Ctrl Pts',(-0.137732458880487,-0.0203383202317681,
0.793603364581467));
#17315=CARTESIAN_POINT('Ctrl Pts',(-0.0575513573065257,-0.126774282767806,
0.801545532704245));
#17316=CARTESIAN_POINT('Ctrl Pts',(0.0753527000357912,-0.117071978271622,
0.809487700827026));
#17317=CARTESIAN_POINT('Ctrl Pts',(0.139225942868322,-0.000119714417332432,
0.817429868949805));
#17318=CARTESIAN_POINT('Ctrl Pts',(0.0755539188089132,0.116942220141962,
0.825372037072586));
#17319=CARTESIAN_POINT('Ctrl Pts',(-0.0573332568284509,0.12687306712048,
0.833314205195366));
#17320=CARTESIAN_POINT('Ctrl Pts',(-0.13769727914169,0.0205751504512258,
0.841256373318145));
#17321=CARTESIAN_POINT('Ctrl Pts',(-0.0919164475821765,-0.104571717796869,
0.849198541440926));
#17322=CARTESIAN_POINT('Ctrl Pts',(0.0380692928980519,-0.133920149482284,
0.857140709563706));
#17323=CARTESIAN_POINT('Ctrl Pts',(0.133179650076608,-0.0405839661022353,
0.865082877686486));
#17324=CARTESIAN_POINT('Ctrl Pts',(0.106283765719693,0.0899312995767124,
0.873025045809266));
#17325=CARTESIAN_POINT('Ctrl Pts',(-0.0179789669825735,0.138060255849953,
0.880967213932046));
#17326=CARTESIAN_POINT('Ctrl Pts',(-0.125771118879347,0.0597118342956578,
0.888909382054826));
#17327=CARTESIAN_POINT('Ctrl Pts',(-0.118344004924669,-0.0733387619032726,
0.896851550177606));
#17328=CARTESIAN_POINT('Ctrl Pts',(-0.00250162451743248,-0.139203517821528,
0.904793718300386));
#17329=CARTESIAN_POINT('Ctrl Pts',(0.115632500949424,-0.0775435504945224,
0.912735886423165));
#17330=CARTESIAN_POINT('Ctrl Pts',(0.127835376168433,0.0551542754370876,
0.920678054545947));
#17331=CARTESIAN_POINT('Ctrl Pts',(0.0229279137899797,0.137325118854324,
0.928620222668725));
#17332=CARTESIAN_POINT('Ctrl Pts',(-0.102983873094174,0.0936920454555137,
0.936562390791507));
#17333=CARTESIAN_POINT('Ctrl Pts',(-0.134551852288801,-0.0357725669300891,
0.944504558914285));
#17334=CARTESIAN_POINT('Ctrl Pts',(-0.0428565117498991,-0.132465832952297,
0.952446727037066));
#17335=CARTESIAN_POINT('Ctrl Pts',(0.0880997963686447,-0.107806787258123,
0.960388895159846));
#17336=CARTESIAN_POINT('Ctrl Pts',(0.138347640177547,0.0156143509765511,
0.968331063282625));
#17337=CARTESIAN_POINT('Ctrl Pts',(0.061854832590724,0.124731139593481,
0.976273231405407));
#17338=CARTESIAN_POINT('Ctrl Pts',(-0.0713033562375951,0.119581390225944,
0.984215399528185));
#17339=CARTESIAN_POINT('Ctrl Pts',(-0.139140345480169,0.00488280234845834,
0.992157567650966));
#17340=CARTESIAN_POINT('Ctrl Pts',(-0.0795104838321055,-0.114288934109561,
1.00009973577375));
#17341=CARTESIAN_POINT('Ctrl Pts',(0.0529591494285269,-0.128760265574912,
1.00804190389653));
#17342=CARTESIAN_POINT('Ctrl Pts',(0.136912761112491,-0.0252739657289669,
1.0159840720193));
#17343=CARTESIAN_POINT('Ctrl Pts',(0.0954402180350474,0.101365883217864,
1.02392624014209));
#17344=CARTESIAN_POINT('Ctrl Pts',(-0.0334653697086341,0.135144169424284,
1.03186840826486));
#17345=CARTESIAN_POINT('Ctrl Pts',(-0.131713240771149,0.0451165125500212,
1.03981057638765));
#17346=CARTESIAN_POINT('Ctrl Pts',(-0.109298251871946,-0.0862425048155002,
1.04775274451043));
#17347=CARTESIAN_POINT('Ctrl Pts',(0.0132451643780021,-0.13859452774087,
1.05569491263321));
#17348=CARTESIAN_POINT('Ctrl Pts',(0.123654649330263,-0.0639797248987874,
1.06363708075599));
#17349=CARTESIAN_POINT('Ctrl Pts',(0.120783771971213,0.0692470788374567,
1.07157924887876));
#17350=CARTESIAN_POINT('Ctrl Pts',(0.00726255089817806,0.139036444335888,
1.07952141700155));
#17351=CARTESIAN_POINT('Ctrl Pts',(-0.112911912907791,0.0814541430660127,
1.08746358512433));
#17352=CARTESIAN_POINT('Ctrl Pts',(-0.129647464608677,-0.0507485213543897,
1.09540575324711));
#17353=CARTESIAN_POINT('Ctrl Pts',(-0.0276126195379174,-0.136460326620484,
1.10334792136989));
#17354=CARTESIAN_POINT('Ctrl Pts',(0.0997182217817603,-0.0971604536002107,
1.11129008949267));
#17355=CARTESIAN_POINT('Ctrl Pts',(0.135696927507188,0.0311483765905046,
1.11923225761545));
#17356=CARTESIAN_POINT('Ctrl Pts',(0.0473633069609982,0.130922093830007,
1.12717442573822));
#17357=CARTESIAN_POINT('Ctrl Pts',(-0.0843599685788644,0.110757722983492,
1.13511659386101));
#17358=CARTESIAN_POINT('Ctrl Pts',(-0.138800846271631,-0.0108721006891078,
1.14305876198379));
#17359=CARTESIAN_POINT('Ctrl Pts',(-0.0660858892268601,-0.122541963197144,
1.15100093010657));
#17360=CARTESIAN_POINT('Ctrl Pts',(0.0671705316110708,-0.121950798202395,
1.15894309822935));
#17361=CARTESIAN_POINT('Ctrl Pts',(0.138891844802359,-0.00964017357273747,
1.16688526635212));
#17362=CARTESIAN_POINT('Ctrl Pts',(0.0833739592533277,0.111501840422208,
1.17482743447491));
#17363=CARTESIAN_POINT('Ctrl Pts',(-0.0485230383040216,0.130496713571114,
1.18276960259768));
#17364=CARTESIAN_POINT('Ctrl Pts',(-0.135967947813762,0.0299431906521225,
1.19071177072047));
#17365=CARTESIAN_POINT('Ctrl Pts',(-0.0988522486080867,-0.0980413710850678,
1.19865393884324));
#17366=CARTESIAN_POINT('Ctrl Pts',(0.0288222657999454,-0.136209964735594,
1.20659610696603));
#17367=CARTESIAN_POINT('Ctrl Pts',(0.130092623711363,-0.0495962373069701,
1.21453827508881));
#17368=CARTESIAN_POINT('Ctrl Pts',(0.112184773380136,0.082452738709893,
1.22248044321158));
#17369=CARTESIAN_POINT('Ctrl Pts',(-0.00849585454694533,0.138966535376798,
1.23042261133437));
#17370=CARTESIAN_POINT('Ctrl Pts',(-0.121393406896754,0.0681727090639588,
1.23836477945715));
#17371=CARTESIAN_POINT('Ctrl Pts',(-0.123082127310551,-0.0650743223999996,
1.24630694757992));
#17372=CARTESIAN_POINT('Ctrl Pts',(-0.0120149744006178,-0.138706589206355,
1.25424911570271));
#17373=CARTESIAN_POINT('Ctrl Pts',(0.110059129405696,-0.0852693704304675,
1.26219128382548));
#17374=CARTESIAN_POINT('Ctrl Pts',(0.13130776387206,0.0462833517151888,
1.27013345194827));
#17375=CARTESIAN_POINT('Ctrl Pts',(0.0322649968732001,0.135435768819968,
1.27807562007105));
#17376=CARTESIAN_POINT('Ctrl Pts',(-0.0963358219719167,0.100515107841202,
1.28601778819382));
#17377=CARTESIAN_POINT('Ctrl Pts',(-0.136683130933199,-0.0264877182308561,
1.29395995631661));
#17378=CARTESIAN_POINT('Ctrl Pts',(-0.0518146499729274,-0.129225073214149,
1.30190212443939));
#17379=CARTESIAN_POINT('Ctrl Pts',(0.0805213734929343,-0.11357898534207,
1.30984429256217));
#17380=CARTESIAN_POINT('Ctrl Pts',(0.1390915465469,0.0061171215252809,1.31778646068495));
#17381=CARTESIAN_POINT('Ctrl Pts',(0.0702395735793815,0.120209316621791,
1.32572862880773));
#17382=CARTESIAN_POINT('Ctrl Pts',(-0.0629590648350173,0.124177428154433,
1.33367079693051));
#17383=CARTESIAN_POINT('Ctrl Pts',(-0.138480731711197,0.0143862582011507,
1.34161296505328));
#17384=CARTESIAN_POINT('Ctrl Pts',(-0.0871398218994898,-0.108584202098263,
1.34955513317607));
#17385=CARTESIAN_POINT('Ctrl Pts',(0.0440301174146577,-0.132080378229483,
1.35749730129884));
#17386=CARTESIAN_POINT('Ctrl Pts',(0.13486394497766,-0.0345773583278084,
1.36543946942163));
#17387=CARTESIAN_POINT('Ctrl Pts',(0.102148545386143,0.0946020732301706,
1.3733816375444));
#17388=CARTESIAN_POINT('Ctrl Pts',(-0.0241454188302812,0.137116288461919,
1.38132380566719));
#17389=CARTESIAN_POINT('Ctrl Pts',(-0.128319693277533,0.0540178939468163,
1.38926597378996));
#17390=CARTESIAN_POINT('Ctrl Pts',(-0.114939956470138,-0.0785664351508689,
1.39720814191275));
#17391=CARTESIAN_POINT('Ctrl Pts',(0.00373660876362508,-0.139175849115243,
1.40515031003553));
#17392=CARTESIAN_POINT('Ctrl Pts',(0.118990018389619,-0.0722858665142316,
1.41309247815831));
#17393=CARTESIAN_POINT('Ctrl Pts',(0.125236419206141,0.0608253567263532,
1.42103464628109));
#17394=CARTESIAN_POINT('Ctrl Pts',(0.0167532566496359,0.13821437898841,
1.42897681440387));
#17395=CARTESIAN_POINT('Ctrl Pts',(-0.107077349343502,0.0889846891406984,
1.43691898252665));
#17396=CARTESIAN_POINT('Ctrl Pts',(-0.132814597987359,-0.0417638487589672,
1.44486115064943));
#17397=CARTESIAN_POINT('Ctrl Pts',(-0.0368790902657646,-0.134252921254984,
1.45280331877221));
#17398=CARTESIAN_POINT('Ctrl Pts',(0.0928396680879532,-0.103751556080299,
1.46074548689499));
#17399=CARTESIAN_POINT('Ctrl Pts',(0.137511141307062,0.0217950526079239,
1.46868765501776));
#17400=CARTESIAN_POINT('Ctrl Pts',(0.0562018483347667,0.127378648737854,
1.47662982314055));
#17401=CARTESIAN_POINT('Ctrl Pts',(-0.0765818961642769,0.116263681173923,
1.48457199126332));
#17402=CARTESIAN_POINT('Ctrl Pts',(-0.13923195096087,-0.00134816270381636,
1.49251415938611));
#17403=CARTESIAN_POINT('Ctrl Pts',(-0.0742871760264013,-0.117748889605885,
1.50045632750888));
#17404=CARTESIAN_POINT('Ctrl Pts',(0.0586284551779338,-0.126233948370975,
1.50839849563167));
#17405=CARTESIAN_POINT('Ctrl Pts',(0.137995068118234,-0.019163470063063,
1.51634066375444));
#17406=CARTESIAN_POINT('Ctrl Pts',(0.0906261803825392,0.105639137646141,
1.52428283187723));
#17407=CARTESIAN_POINT('Ctrl Pts',(0.00417072711528833,0.124051375507138,
1.52957761062575));
#17408=CARTESIAN_POINT('Ctrl Pts',(-0.0334019664627544,0.1129391839063,
1.53222500000001));
#17409=CARTESIAN_POINT('Ctrl Pts',(-0.0551480035117261,0.114734422509858,
-0.0109985226280628));
#17410=CARTESIAN_POINT('Ctrl Pts',(-0.093317938433455,0.0963877427684319,
-0.00835113325380276));
#17411=CARTESIAN_POINT('Ctrl Pts',(-0.149247407742026,0.0189255452031589,
-0.00305635450528277));
#17412=CARTESIAN_POINT('Ctrl Pts',(-0.0966876253720675,-0.115446371588928,
0.00488581361749726));
#17413=CARTESIAN_POINT('Ctrl Pts',(0.0445747075563756,-0.143685636564375,
0.0128279817402772));
#17414=CARTESIAN_POINT('Ctrl Pts',(0.144936900801175,-0.0404809362687151,
0.0207701498630572));
#17415=CARTESIAN_POINT('Ctrl Pts',(0.112556116319125,0.0999057960529736,
0.0287123179858373));
#17416=CARTESIAN_POINT('Ctrl Pts',(-0.0229555792165621,0.148717415239805,
0.0366544861086172));
#17417=CARTESIAN_POINT('Ctrl Pts',(-0.137428156769908,0.0613155244327884,
0.0445966542313972));
#17418=CARTESIAN_POINT('Ctrl Pts',(-0.126007400730642,-0.0822718633254329,
0.0525388223541772));
#17419=CARTESIAN_POINT('Ctrl Pts',(0.000851700720621877,-0.150482305134309,
0.0604809904769572));
#17420=CARTESIAN_POINT('Ctrl Pts',(0.126929176276611,-0.0808394286734405,
0.0684231585997372));
#17421=CARTESIAN_POINT('Ctrl Pts',(0.136727213562698,0.0628627408439891,
0.0763653267225173));
#17422=CARTESIAN_POINT('Ctrl Pts',(0.0212686937255662,0.148975090584026,
0.0843074948452972));
#17423=CARTESIAN_POINT('Ctrl Pts',(-0.113673932864549,0.0986115272026031,
0.0922496629680772));
#17424=CARTESIAN_POINT('Ctrl Pts',(-0.144479665027646,-0.0420906285100245,
0.100191831090857));
#17425=CARTESIAN_POINT('Ctrl Pts',(-0.0429271251068198,-0.144233284958223,
0.108133999213637));
#17426=CARTESIAN_POINT('Ctrl Pts',(0.0979510420095061,-0.114243518700172,
0.116076167336417));
#17427=CARTESIAN_POINT('Ctrl Pts',(0.149096007275942,0.0204050915936607,
0.124018335459197));
#17428=CARTESIAN_POINT('Ctrl Pts',(0.0636537044864716,0.136360518400275,
0.131960503581977));
#17429=CARTESIAN_POINT('Ctrl Pts',(-0.0801019266996435,0.127395713772213,
0.139902671704757));
#17430=CARTESIAN_POINT('Ctrl Pts',(-0.15047596611352,0.00172334100814176,
0.147844839827537));
#17431=CARTESIAN_POINT('Ctrl Pts',(-0.0829985603893774,-0.125527785761544,
0.155787007950317));
#17432=CARTESIAN_POINT('Ctrl Pts',(0.0605140527882773,-0.137782566606816,
0.163729176073097));
#17433=CARTESIAN_POINT('Ctrl Pts',(0.148589577098441,-0.0238143605552183,
0.171671344195877));
#17434=CARTESIAN_POINT('Ctrl Pts',(0.100541783424623,0.111970245809892,
0.179613512318657));
#17435=CARTESIAN_POINT('Ctrl Pts',(-0.0396126128240685,0.145178604134651,
0.187555680441437));
#17436=CARTESIAN_POINT('Ctrl Pts',(-0.143477786216001,0.0453884461694337,
0.195497848564217));
#17437=CARTESIAN_POINT('Ctrl Pts',(-0.115902567375552,-0.095982191346566,
0.203440016686997));
#17438=CARTESIAN_POINT('Ctrl Pts',(0.0178513102906219,-0.149423281002214,
0.211382184809777));
#17439=CARTESIAN_POINT('Ctrl Pts',(0.135251553802876,-0.0659772944027704,
0.219324352932557));
#17440=CARTESIAN_POINT('Ctrl Pts',(0.128747479107914,0.07791067196398,0.227266521055337));
#17441=CARTESIAN_POINT('Ctrl Pts',(0.00429748682099232,0.150424458749874,
0.235208689178117));
#17442=CARTESIAN_POINT('Ctrl Pts',(-0.124089444892588,0.0851339876261335,
0.243150857300897));
#17443=CARTESIAN_POINT('Ctrl Pts',(-0.138797696890977,-0.0581479623084488,
0.251093025423677));
#17444=CARTESIAN_POINT('Ctrl Pts',(-0.0263529993083425,-0.148160405002171,
0.259035193546457));
#17445=CARTESIAN_POINT('Ctrl Pts',(0.110233752987369,-0.102442695616748,
0.266977361669237));
#17446=CARTESIAN_POINT('Ctrl Pts',(0.145835062802846,0.0371230472913779,
0.274919529792017));
#17447=CARTESIAN_POINT('Ctrl Pts',(0.0478364728857143,0.142680265085169,
0.282861697914797));
#17448=CARTESIAN_POINT('Ctrl Pts',(-0.0939852406223356,0.117527701960322,
0.290803866037577));
#17449=CARTESIAN_POINT('Ctrl Pts',(-0.14970681824969,-0.01529231023972,
0.298746034160357));
#17450=CARTESIAN_POINT('Ctrl Pts',(-0.0682815703945392,-0.134102995221473,
0.306688202283137));
#17451=CARTESIAN_POINT('Ctrl Pts',(0.0756966107742644,-0.1300615596562,
0.314630370405917));
#17452=CARTESIAN_POINT('Ctrl Pts',(0.150328919865546,-0.00687037371415525,
0.322572538528697));
#17453=CARTESIAN_POINT('Ctrl Pts',(0.0872444944832666,0.122614780370367,
0.330514706651477));
#17454=CARTESIAN_POINT('Ctrl Pts',(-0.0557648508131485,0.139772198940638,
0.338456874774257));
#17455=CARTESIAN_POINT('Ctrl Pts',(-0.147687863823926,0.0288839239377102,
0.346399042897038));
#17456=CARTESIAN_POINT('Ctrl Pts',(-0.104313621021262,-0.10846499275041,
0.354341211019817));
#17457=CARTESIAN_POINT('Ctrl Pts',(0.0346226151823369,-0.146448833047075,
0.362283379142597));
#17458=CARTESIAN_POINT('Ctrl Pts',(0.141840978962514,-0.0502704970123603,
0.370225547265377));
#17459=CARTESIAN_POINT('Ctrl Pts',(0.119118434135606,0.0919607787700563,
0.378167715388157));
#17460=CARTESIAN_POINT('Ctrl Pts',(-0.0127288338612142,0.149946533709345,
0.386109883510937));
#17461=CARTESIAN_POINT('Ctrl Pts',(-0.132915182358376,0.070565859178174,
0.394052051633717));
#17462=CARTESIAN_POINT('Ctrl Pts',(-0.131337568919768,-0.0734603918663599,
0.401994219756497));
#17463=CARTESIAN_POINT('Ctrl Pts',(-0.00944124952954395,-0.150189377088511,
0.409936387879277));
#17464=CARTESIAN_POINT('Ctrl Pts',(0.121104224366159,-0.0893294633566384,
0.417878556002057));
#17465=CARTESIAN_POINT('Ctrl Pts',(0.140705787232781,0.0533654159743681,
0.425820724124838));
#17466=CARTESIAN_POINT('Ctrl Pts',(0.0314063937394313,0.147172091835368,
0.433762892247617));
#17467=CARTESIAN_POINT('Ctrl Pts',(-0.106664482920656,0.106154012011714,
0.441705060370398));
#17468=CARTESIAN_POINT('Ctrl Pts',(-0.147019735166745,-0.032112048430678,
0.449647228493177));
#17469=CARTESIAN_POINT('Ctrl Pts',(-0.052689806088835,-0.14096017351449,
0.457589396615958));
#17470=CARTESIAN_POINT('Ctrl Pts',(0.0899093983958942,-0.120674298270189,
0.465531564738737));
#17471=CARTESIAN_POINT('Ctrl Pts',(0.15014235720654,0.0101616315312987,
0.473473732861518));
#17472=CARTESIAN_POINT('Ctrl Pts',(0.0728294921055832,0.131688462906045,
0.481415900984297));
#17473=CARTESIAN_POINT('Ctrl Pts',(-0.071202669822089,0.132575133389036,
0.489358069107078));
#17474=CARTESIAN_POINT('Ctrl Pts',(-0.150005871264529,0.012009361726732,
0.497300237229857));
#17475=CARTESIAN_POINT('Ctrl Pts',(-0.0913882839399832,-0.119558219045865,
0.505242405352637));
#17476=CARTESIAN_POINT('Ctrl Pts',(0.0509503601487159,-0.141598188489932,
0.513184573475417));
#17477=CARTESIAN_POINT('Ctrl Pts',(0.146613240011817,-0.0339196703426114,
0.521126741598197));
#17478=CARTESIAN_POINT('Ctrl Pts',(0.107963329873666,0.104832750538675,
0.529068909720978));
#17479=CARTESIAN_POINT('Ctrl Pts',(-0.0295920819230583,0.147547602048875,
0.537011077843756));
#17480=CARTESIAN_POINT('Ctrl Pts',(-0.140038106568177,0.055093691941219,
0.544953245966537));
#17481=CARTESIAN_POINT('Ctrl Pts',(-0.122194838935542,-0.0878316999746162,
0.552895414089317));
#17482=CARTESIAN_POINT('Ctrl Pts',(0.00759145471482065,-0.150294231420327,
0.560837582212097));
#17483=CARTESIAN_POINT('Ctrl Pts',(0.130423195946632,-0.0750718065719766,
0.568779750334878));
#17484=CARTESIAN_POINT('Ctrl Pts',(0.133773890807325,0.0689241055160235,
0.576721918457657));
#17485=CARTESIAN_POINT('Ctrl Pts',(0.0145739585745413,0.149778456108953,
0.584664086580438));
#17486=CARTESIAN_POINT('Ctrl Pts',(-0.117977216952174,0.0934203535806499,
0.592606254703216));
#17487=CARTESIAN_POINT('Ctrl Pts',(-0.142449141490696,-0.0485203902651028,
0.600548422825998));
#17488=CARTESIAN_POINT('Ctrl Pts',(-0.036423018067407,-0.146011471938939,
0.608490590948776));
#17489=CARTESIAN_POINT('Ctrl Pts',(0.102970331784443,-0.109741044988262,
0.616432759071558));
#17490=CARTESIAN_POINT('Ctrl Pts',(0.148032279177632,0.0270634532975707,
0.624374927194337));
#17491=CARTESIAN_POINT('Ctrl Pts',(0.0574814509102497,0.139075048028633,
0.632317095317117));
#17492=CARTESIAN_POINT('Ctrl Pts',(-0.0857282916847416,0.123679611042927,
0.640259263439898));
#17493=CARTESIAN_POINT('Ctrl Pts',(-0.150402111894479,-0.00501905574730406,
0.648201431562677));
#17494=CARTESIAN_POINT('Ctrl Pts',(-0.0772921462128499,-0.129119751845818,
0.656143599685457));
#17495=CARTESIAN_POINT('Ctrl Pts',(0.0666253659236285,-0.134933490277457,
0.664085767808237));
#17496=CARTESIAN_POINT('Ctrl Pts',(0.14950719819016,-0.0171342893707992,
0.672027935931017));
#17497=CARTESIAN_POINT('Ctrl Pts',(0.0954250774564579,0.11636168087194,
0.679970104053797));
#17498=CARTESIAN_POINT('Ctrl Pts',(-0.0460762176180427,0.143258397146306,
0.687912272176577));
#17499=CARTESIAN_POINT('Ctrl Pts',(-0.145366963764729,0.0389157041403328,
0.695854440299358));
#17500=CARTESIAN_POINT('Ctrl Pts',(-0.111486636987321,-0.101077771820372,
0.703796608422136));
#17501=CARTESIAN_POINT('Ctrl Pts',(0.02452690272786,-0.148473624679578,
0.711738776544918));
#17502=CARTESIAN_POINT('Ctrl Pts',(0.138071279799868,-0.0598523840572839,
0.719680944667696));
#17503=CARTESIAN_POINT('Ctrl Pts',(0.125128179973684,0.0835997892305201,
0.727623112790477));
#17504=CARTESIAN_POINT('Ctrl Pts',(-0.00244518761474098,0.150465967050502,
0.735565280913257));
#17505=CARTESIAN_POINT('Ctrl Pts',(-0.127778512144395,0.0794898610961098,
0.743507449036036));
#17506=CARTESIAN_POINT('Ctrl Pts',(-0.136053592364468,-0.0643071239260258,
0.751449617158818));
#17507=CARTESIAN_POINT('Ctrl Pts',(-0.019689604662082,-0.149192176910068,
0.759391785281597));
#17508=CARTESIAN_POINT('Ctrl Pts',(0.114712083700712,-0.0974018687498071,
0.767333953404378));
#17509=CARTESIAN_POINT('Ctrl Pts',(0.144025718573537,0.0436185576594447,
0.775276121527157));
#17510=CARTESIAN_POINT('Ctrl Pts',(0.0413969989087525,0.14467990414796,
0.783218289649938));
#17511=CARTESIAN_POINT('Ctrl Pts',(-0.0991556246317344,0.113199594905656,
0.791160457772717));
#17512=CARTESIAN_POINT('Ctrl Pts',(-0.148871509365196,-0.021983172706469,
0.799102625895497));
#17513=CARTESIAN_POINT('Ctrl Pts',(-0.062205797368885,-0.137027095702329,
0.807044794018277));
#17514=CARTESIAN_POINT('Ctrl Pts',(0.081446815661698,-0.126540121706451,
0.814986962141057));
#17515=CARTESIAN_POINT('Ctrl Pts',(0.150485778196879,-0.000129396266831759,
0.822929130263837));
#17516=CARTESIAN_POINT('Ctrl Pts',(0.0816643079123276,0.126399869446589,
0.830871298386618));
#17517=CARTESIAN_POINT('Ctrl Pts',(-0.0619700581130299,0.137133869194964,
0.838813466509397));
#17518=CARTESIAN_POINT('Ctrl Pts',(-0.148833484480893,0.0222391564630926,
0.846755634632177));
#17519=CARTESIAN_POINT('Ctrl Pts',(-0.0993501488194509,-0.113028908304323,
0.854697802754957));
#17520=CARTESIAN_POINT('Ctrl Pts',(0.041148129789194,-0.144750881164039,
0.862639970877736));
#17521=CARTESIAN_POINT('Ctrl Pts',(0.143950494202948,-0.0438661760544617,
0.870582139000517));
#17522=CARTESIAN_POINT('Ctrl Pts',(0.114879417330645,0.0972044528644933,
0.878524307123298));
#17523=CARTESIAN_POINT('Ctrl Pts',(-0.0194330078274841,0.149225816766708,
0.886466475246077));
#17524=CARTESIAN_POINT('Ctrl Pts',(-0.135942801386891,0.0645410019599824,
0.894408643368857));
#17525=CARTESIAN_POINT('Ctrl Pts',(-0.127915022941288,-0.0792700011911429,
0.902350811491637));
#17526=CARTESIAN_POINT('Ctrl Pts',(-0.00270394227186439,-0.150461539534541,
0.910292979614417));
#17527=CARTESIAN_POINT('Ctrl Pts',(0.124984227305131,-0.0838148501630433,
0.918235147737197));
#17528=CARTESIAN_POINT('Ctrl Pts',(0.138174004553101,0.0596148525845174,
0.926177315859977));
#17529=CARTESIAN_POINT('Ctrl Pts',(0.0247821984756025,0.148431225898158,
0.934119483982757));
#17530=CARTESIAN_POINT('Ctrl Pts',(-0.11131264737753,0.101269347369872,
0.942061652105537));
#17531=CARTESIAN_POINT('Ctrl Pts',(-0.145433672650089,-0.0386656571445607,
0.950003820228317));
#17532=CARTESIAN_POINT('Ctrl Pts',(-0.0463225128062989,-0.143178947440692,
0.957945988351097));
#17533=CARTESIAN_POINT('Ctrl Pts',(0.0952248276606132,-0.116525612549003,
0.965888156473877));
#17534=CARTESIAN_POINT('Ctrl Pts',(0.149536443172165,0.0168771545685866,
0.973830324596656));
#17535=CARTESIAN_POINT('Ctrl Pts',(0.0668573142755158,0.134818714245386,
0.981772492719438));
#17536=CARTESIAN_POINT('Ctrl Pts',(-0.0770699830103684,0.129252481220654,
0.989714660842216));
#17537=CARTESIAN_POINT('Ctrl Pts',(-0.15039325815857,0.00527769678589187,
0.997656828964997));
#17538=CARTESIAN_POINT('Ctrl Pts',(-0.0859408583470751,-0.123532000103139,
1.00559899708778));
#17539=CARTESIAN_POINT('Ctrl Pts',(0.0572421967501742,-0.139173693973137,
1.01354116521056));
#17540=CARTESIAN_POINT('Ctrl Pts',(0.147985518909957,-0.0273179863069172,
1.02148333333334));
#17541=CARTESIAN_POINT('Ctrl Pts',(0.103158902618224,0.109563803299803,
1.02942550145612));
#17542=CARTESIAN_POINT('Ctrl Pts',(-0.0361718663885326,0.146073893166727,
1.0373676695789));
#17543=CARTESIAN_POINT('Ctrl Pts',(-0.142365489706367,0.0487652901517079,
1.04530983770168));
#17544=CARTESIAN_POINT('Ctrl Pts',(-0.118137698690712,-0.0932173284908804,
1.05325200582446));
#17545=CARTESIAN_POINT('Ctrl Pts',(0.0143163610725534,-0.149803297655807,
1.06119417394724));
#17546=CARTESIAN_POINT('Ctrl Pts',(0.133655163317704,-0.0691540562905145,
1.06913634207002));
#17547=CARTESIAN_POINT('Ctrl Pts',(0.130552105047211,0.0748474051030229,
1.0770785101928));
#17548=CARTESIAN_POINT('Ctrl Pts',(0.0078499064261323,0.150280954056111,
1.08502067831558));
#17549=CARTESIAN_POINT('Ctrl Pts',(-0.122043612932812,0.0880417101447944,
1.09296284643836));
#17550=CARTESIAN_POINT('Ctrl Pts',(-0.140132644828567,-0.0548527851276936,
1.10090501456114));
#17551=CARTESIAN_POINT('Ctrl Pts',(-0.0298457776877653,-0.147496493982489,
1.10884718268392));
#17552=CARTESIAN_POINT('Ctrl Pts',(0.107782887988268,-0.10501826145877,
1.1167893508067));
#17553=CARTESIAN_POINT('Ctrl Pts',(0.146671355310253,0.033667487497105,
1.12473151892948));
#17554=CARTESIAN_POINT('Ctrl Pts',(0.0511937930472066,0.141510359113225,
1.13267368705226));
#17555=CARTESIAN_POINT('Ctrl Pts',(-0.0911825429852659,0.119715203870077,
1.14061585517504));
#17556=CARTESIAN_POINT('Ctrl Pts',(-0.150026302104679,-0.0117513769282424,
1.14855802329782));
#17557=CARTESIAN_POINT('Ctrl Pts',(-0.0714305557085884,-0.132452489195471,
1.1565001914206));
#17558=CARTESIAN_POINT('Ctrl Pts',(0.0726029180563751,-0.131813513998426,
1.16444235954338));
#17559=CARTESIAN_POINT('Ctrl Pts',(0.150124660100533,-0.010419818262018,
1.17238452766616));
#17560=CARTESIAN_POINT('Ctrl Pts',(0.0901167906002831,0.120519501471002,
1.18032669578894));
#17561=CARTESIAN_POINT('Ctrl Pts',(-0.0524473171394798,0.141050576417769,
1.18826886391172));
#17562=CARTESIAN_POINT('Ctrl Pts',(-0.146964294261872,0.0323648326895764,
1.1962110320345));
#17563=CARTESIAN_POINT('Ctrl Pts',(-0.106846879624786,-0.105970422747861,
1.20415320015727));
#17564=CARTESIAN_POINT('Ctrl Pts',(0.0311532535456026,-0.14722588419309,
1.21209536828006));
#17565=CARTESIAN_POINT('Ctrl Pts',(0.140613805972886,-0.0536073106276968,
1.22003753640283));
#17566=CARTESIAN_POINT('Ctrl Pts',(0.121257666323848,0.0891210667609394,
1.22797970452562));
#17567=CARTESIAN_POINT('Ctrl Pts',(-0.00918295295119051,0.150205391241489,
1.2359218726484));
#17568=CARTESIAN_POINT('Ctrl Pts',(-0.131211043922368,0.0736861461587066,
1.24386404077118));
#17569=CARTESIAN_POINT('Ctrl Pts',(-0.133036338837895,-0.0703371788708997,
1.25180620889396));
#17570=CARTESIAN_POINT('Ctrl Pts',(-0.0129866800356469,-0.149924422041766,
1.25974837701674));
#17571=CARTESIAN_POINT('Ctrl Pts',(0.118960111851797,-0.0921654923014072,
1.26769054513952));
#17572=CARTESIAN_POINT('Ctrl Pts',(0.141927220045961,0.050026496908035,
1.2756327132623));
#17573=CARTESIAN_POINT('Ctrl Pts',(0.0348744139414821,0.146389075532006,
1.28357488138508));
#17574=CARTESIAN_POINT('Ctrl Pts',(-0.104126938119509,0.108644221848311,
1.29151704950786));
#17575=CARTESIAN_POINT('Ctrl Pts',(-0.147737317493493,-0.0286299004949125,
1.29945921763064));
#17576=CARTESIAN_POINT('Ctrl Pts',(-0.0560051364173496,-0.139676092720537,
1.30740138575342));
#17577=CARTESIAN_POINT('Ctrl Pts',(0.0870335032532438,-0.122764634549313,
1.3153435538762));
#17578=CARTESIAN_POINT('Ctrl Pts',(0.150340512633584,0.00661184096937889,
1.32328572199898));
#17579=CARTESIAN_POINT('Ctrl Pts',(0.0759201674095095,0.129931190880528,
1.33122789012176));
#17580=CARTESIAN_POINT('Ctrl Pts',(-0.0680508508044829,0.134220221643466,
1.33917005824454));
#17581=CARTESIAN_POINT('Ctrl Pts',(-0.149680298423566,0.0155497403439283,
1.34711222636732));
#17582=CARTESIAN_POINT('Ctrl Pts',(-0.0941872156892785,-0.117365900463673,
1.3550543944901));
#17583=CARTESIAN_POINT('Ctrl Pts',(0.0475910332998192,-0.142762319241037,
1.36299656261288));
#17584=CARTESIAN_POINT('Ctrl Pts',(0.145771005694385,-0.0373737865856905,
1.37093873073566));
#17585=CARTESIAN_POINT('Ctrl Pts',(0.110409762917901,0.10225297323032,1.37888089885844));
#17586=CARTESIAN_POINT('Ctrl Pts',(-0.0260981686868614,0.148205506441964,
1.38682306698121));
#17587=CARTESIAN_POINT('Ctrl Pts',(-0.138697490589939,0.0583865667538053,
1.394765235104));
#17588=CARTESIAN_POINT('Ctrl Pts',(-0.124235673603468,-0.0849204601545819,
1.40270740322677));
#17589=CARTESIAN_POINT('Ctrl Pts',(0.0040388053119065,-0.150431633134115,
1.41064957134956));
#17590=CARTESIAN_POINT('Ctrl Pts',(0.12861328245382,-0.0781319533624403,
1.41859173947234));
#17591=CARTESIAN_POINT('Ctrl Pts',(0.1353648581188,0.0657445800149866,1.42653390759512));
#17592=CARTESIAN_POINT('Ctrl Pts',(0.0181081687242482,0.149392404544468,
1.43447607571789));
#17593=CARTESIAN_POINT('Ctrl Pts',(-0.115737181672069,0.0961812857364522,
1.44241824384068));
#17594=CARTESIAN_POINT('Ctrl Pts',(-0.143555918690644,-0.0451414811888502,
1.45036041196346));
#17595=CARTESIAN_POINT('Ctrl Pts',(-0.0398616700558823,-0.145110565703753,
1.45830258008624));
#17596=CARTESIAN_POINT('Ctrl Pts',(0.100348034367198,-0.112142416378873,
1.46624474820902));
#17597=CARTESIAN_POINT('Ctrl Pts',(0.14863229283285,0.0235577176564554,
1.4741869163318));
#17598=CARTESIAN_POINT('Ctrl Pts',(0.0607471474677608,0.137680339497592,
1.48212908445458));
#17599=CARTESIAN_POINT('Ctrl Pts',(-0.0827754224726193,0.125666453945577,
1.49007125257736));
#17600=CARTESIAN_POINT('Ctrl Pts',(-0.150492272191201,-0.00145719475437189,
1.49801342070014));
#17601=CARTESIAN_POINT('Ctrl Pts',(-0.0802951178786721,-0.12727177793954,
1.50595558882292));
#17602=CARTESIAN_POINT('Ctrl Pts',(0.0633700050447994,-0.136443062004882,
1.5138977569457));
#17603=CARTESIAN_POINT('Ctrl Pts',(0.149155357006591,-0.0207133070603065,
1.52183992506848));
#17604=CARTESIAN_POINT('Ctrl Pts',(0.0979555318420461,0.114182655252422,
1.52978209319126));
#17605=CARTESIAN_POINT('Ctrl Pts',(0.00450803278943675,0.134083974545181,
1.53507687193978));
#17606=CARTESIAN_POINT('Ctrl Pts',(-0.0361033354337414,0.122073089461022,
1.53772426131404));
#17607=CARTESIAN_POINT('Ctrl Pts',(-0.0592743564846203,0.123319225136773,
-0.00549926131403157));
#17608=CARTESIAN_POINT('Ctrl Pts',(-0.100300290071938,0.10359978715075,
-0.00285187193977157));
#17609=CARTESIAN_POINT('Ctrl Pts',(-0.160414584165772,0.0203416160441626,
0.00244290680874841));
#17610=CARTESIAN_POINT('Ctrl Pts',(-0.103922107946056,-0.124084444561314,
0.0103850749315284));
#17611=CARTESIAN_POINT('Ctrl Pts',(0.0479099321398382,-0.154436663180837,
0.0183272430543084));
#17612=CARTESIAN_POINT('Ctrl Pts',(0.155781551077148,-0.0435098515708298,
0.0262694111770884));
#17613=CARTESIAN_POINT('Ctrl Pts',(0.120977930992648,0.107381072623318,
0.0342115792998684));
#17614=CARTESIAN_POINT('Ctrl Pts',(-0.0246731903087699,0.159844935900913,
0.0421537474226484));
#17615=CARTESIAN_POINT('Ctrl Pts',(-0.147710978397823,0.0659033513787588,
0.0500959155454284));
#17616=CARTESIAN_POINT('Ctrl Pts',(-0.135435684249567,-0.0884277117007276,
0.0580380836682085));
#17617=CARTESIAN_POINT('Ctrl Pts',(0.000915427738408385,-0.16174188059703,
0.0659802517909884));
#17618=CARTESIAN_POINT('Ctrl Pts',(0.13642643003965,-0.0868880976295618,
0.0739224199137684));
#17619=CARTESIAN_POINT('Ctrl Pts',(0.146957588340267,0.0675663355536457,
0.0818645880365484));
#17620=CARTESIAN_POINT('Ctrl Pts',(0.0228600865593111,0.160121891352391,
0.0898067561593285));
#17621=CARTESIAN_POINT('Ctrl Pts',(-0.122179386207322,0.105989962368389,
0.0977489242821083));
#17622=CARTESIAN_POINT('Ctrl Pts',(-0.155290103436038,-0.0452399862206161,
0.105691092404888));
#17623=CARTESIAN_POINT('Ctrl Pts',(-0.0461390722131997,-0.155025288408554,
0.113633260527668));
#17624=CARTESIAN_POINT('Ctrl Pts',(0.105280057525145,-0.122791590307548,
0.121575428650448));
#17625=CARTESIAN_POINT('Ctrl Pts',(0.160251855424436,0.0219318669073289,
0.129517596773229));
#17626=CARTESIAN_POINT('Ctrl Pts',(0.0684164816681947,0.146563455853242,
0.137459764896008));
#17627=CARTESIAN_POINT('Ctrl Pts',(-0.086095413359615,0.136927875387926,
0.145401933018789));
#17628=CARTESIAN_POINT('Ctrl Pts',(-0.16173506727009,0.00185228698694943,
0.153344101141568));
#17629=CARTESIAN_POINT('Ctrl Pts',(-0.0892087826023274,-0.134920182928699,
0.161286269264348));
#17630=CARTESIAN_POINT('Ctrl Pts',(0.0650419110192955,-0.148091906331324,
0.169228437387128));
#17631=CARTESIAN_POINT('Ctrl Pts',(0.159707532494063,-0.025596228460074,
0.177170605509908));
#17632=CARTESIAN_POINT('Ctrl Pts',(0.108064646638443,0.120348223746572,
0.185112773632688));
#17633=CARTESIAN_POINT('Ctrl Pts',(-0.0425765573421325,0.156041339440091,
0.193054941755468));
#17634=CARTESIAN_POINT('Ctrl Pts',(-0.154213260793436,0.0487845573223287,
0.200997109878248));
#17635=CARTESIAN_POINT('Ctrl Pts',(-0.124574774400312,-0.103163891052585,
0.208939278001028));
#17636=CARTESIAN_POINT('Ctrl Pts',(0.0191870033818907,-0.160603616835255,
0.216881446123808));
#17637=CARTESIAN_POINT('Ctrl Pts',(0.145371514918136,-0.0709139301387177,
0.224823614246588));
#17638=CARTESIAN_POINT('Ctrl Pts',(0.138380784202201,0.0837402018183176,
0.232765782369368));
#17639=CARTESIAN_POINT('Ctrl Pts',(0.00461903876105218,0.161679705957985,
0.240707950492149));
#17640=CARTESIAN_POINT('Ctrl Pts',(-0.133374220718213,0.0915039894496894,
0.248650118614928));
#17641=CARTESIAN_POINT('Ctrl Pts',(-0.149182991964712,-0.0624987819548612,
0.256592286737709));
#17642=CARTESIAN_POINT('Ctrl Pts',(-0.0283248164207669,-0.159246248345813,
0.264534454860488));
#17643=CARTESIAN_POINT('Ctrl Pts',(0.118481800883715,-0.110107791262854,
0.272476622983269));
#17644=CARTESIAN_POINT('Ctrl Pts',(0.156746916480749,0.0399007144198201,
0.280418791106048));
#17645=CARTESIAN_POINT('Ctrl Pts',(0.0514157533588968,0.153356066537929,
0.288360959228829));
#17646=CARTESIAN_POINT('Ctrl Pts',(-0.101017521980764,0.126321506839912,
0.296303127351608));
#17647=CARTESIAN_POINT('Ctrl Pts',(-0.160908369261695,-0.0164365306249019,
0.304245295474388));
#17648=CARTESIAN_POINT('Ctrl Pts',(-0.0733906195540655,-0.144137017448375,
0.312187463597168));
#17649=CARTESIAN_POINT('Ctrl Pts',(0.0813604773699057,-0.13979318853071,
0.320129631719948));
#17650=CARTESIAN_POINT('Ctrl Pts',(0.161577018543625,-0.00738443741900211,
0.328071799842729));
#17651=CARTESIAN_POINT('Ctrl Pts',(0.0937724112935796,0.131789217000595,
0.336013967965508));
#17652=CARTESIAN_POINT('Ctrl Pts',(-0.0599373583072218,0.150230409426965,
0.343956136088289));
#17653=CARTESIAN_POINT('Ctrl Pts',(-0.158738350099833,0.0310451130618767,
0.351898304211068));
#17654=CARTESIAN_POINT('Ctrl Pts',(-0.112118705390683,-0.116580696253536,
0.359840472333849));
#17655=CARTESIAN_POINT('Ctrl Pts',(0.0372131918485748,-0.15740661101073,
0.367782640456628));
#17656=CARTESIAN_POINT('Ctrl Pts',(0.152453982298084,-0.0540318990865351,
0.375724808579408));
#17657=CARTESIAN_POINT('Ctrl Pts',(0.128031262769868,0.0988415833088236,
0.383666976702188));
#17658=CARTESIAN_POINT('Ctrl Pts',(-0.0136812466069205,0.161166021011634,
0.391609144824968));
#17659=CARTESIAN_POINT('Ctrl Pts',(-0.142860328563903,0.0758458262533652,
0.399551312947749));
#17660=CARTESIAN_POINT('Ctrl Pts',(-0.141164672957165,-0.0789569372907697,
0.407493481070528));
#17661=CARTESIAN_POINT('Ctrl Pts',(-0.0101476745237983,-0.161427034722196,
0.415435649193308));
#17662=CARTESIAN_POINT('Ctrl Pts',(0.130165636283581,-0.0960133843187101,
0.423377817316089));
#17663=CARTESIAN_POINT('Ctrl Pts',(0.151233851831306,0.0573583899504574,
0.431319985438868));
#17664=CARTESIAN_POINT('Ctrl Pts',(0.0337563222576384,0.158183986373718,
0.439262153561649));
#17665=CARTESIAN_POINT('Ctrl Pts',(-0.114645466422773,0.114096800420287,
0.447204321684428));
#17666=CARTESIAN_POINT('Ctrl Pts',(-0.158020229883659,-0.0345147763277912,
0.455146489807208));
#17667=CARTESIAN_POINT('Ctrl Pts',(-0.0566322287360923,-0.151507272121918,
0.463088657929988));
#17668=CARTESIAN_POINT('Ctrl Pts',(0.0966367119836487,-0.129703541718919,
0.471030826052768));
#17669=CARTESIAN_POINT('Ctrl Pts',(0.161376496659739,0.0109219578497271,
0.478972994175549));
#17670=CARTESIAN_POINT('Ctrl Pts',(0.0782788315581001,0.141541821972661,
0.486915162298328));
#17671=CARTESIAN_POINT('Ctrl Pts',(-0.0765302851406724,0.142494836024782,
0.494857330421108));
#17672=CARTESIAN_POINT('Ctrl Pts',(-0.161229798395673,0.0129079412274925,
0.502799498543889));
#17673=CARTESIAN_POINT('Ctrl Pts',(-0.0982262525537151,-0.128503953817366,
0.510741666666668));
#17674=CARTESIAN_POINT('Ctrl Pts',(0.0547626317937811,-0.152193025452748,
0.518683834789449));
#17675=CARTESIAN_POINT('Ctrl Pts',(0.157583319439253,-0.0364576503898468,
0.526626002912228));
#17676=CARTESIAN_POINT('Ctrl Pts',(0.116041497328862,0.112676677866884,
0.534568171035008));
#17677=CARTESIAN_POINT('Ctrl Pts',(-0.0318062577307366,0.158587593482618,
0.542510339157789));
#17678=CARTESIAN_POINT('Ctrl Pts',(-0.150516213127973,0.0592159811457737,
0.550452507280567));
#17679=CARTESIAN_POINT('Ctrl Pts',(-0.131337854181896,-0.0944035534094825,
0.558394675403349));
#17680=CARTESIAN_POINT('Ctrl Pts',(0.00815947204521347,-0.161539734596121,
0.566336843526128));
#17681=CARTESIAN_POINT('Ctrl Pts',(0.140181883624494,-0.080688923285235,
0.574279011648909));
#17682=CARTESIAN_POINT('Ctrl Pts',(0.143783288371658,0.0740812312429708,
0.582221179771688));
#17683=CARTESIAN_POINT('Ctrl Pts',(0.0156644295519346,0.160985367298567,
0.590163347894469));
#17684=CARTESIAN_POINT('Ctrl Pts',(-0.126804656005353,0.100410368253513,
0.598105516017247));
#17685=CARTESIAN_POINT('Ctrl Pts',(-0.153107649524464,-0.0521508436608248,
0.606047684140029));
#17686=CARTESIAN_POINT('Ctrl Pts',(-0.0391483067326994,-0.156936525122116,
0.613989852262808));
#17687=CARTESIAN_POINT('Ctrl Pts',(0.110674906884577,-0.117952226869747,
0.621932020385589));
#17688=CARTESIAN_POINT('Ctrl Pts',(0.159108535730396,0.0290884288879846,
0.629874188508368));
#17689=CARTESIAN_POINT('Ctrl Pts',(0.061782400006242,0.14948109541648,0.637816356631148));
#17690=CARTESIAN_POINT('Ctrl Pts',(-0.0921427612707386,0.132933721767072,
0.645758524753929));
#17691=CARTESIAN_POINT('Ctrl Pts',(-0.161655687038194,-0.0053945978210935,
0.653700692876707));
#17692=CARTESIAN_POINT('Ctrl Pts',(-0.0830753959589387,-0.138780911597048,
0.661642860999489));
#17693=CARTESIAN_POINT('Ctrl Pts',(0.0716104924784035,-0.145029652845349,
0.669585029122267));
#17694=CARTESIAN_POINT('Ctrl Pts',(0.160693812980115,-0.0184163326249747,
0.677527197245049));
#17695=CARTESIAN_POINT('Ctrl Pts',(0.102565092089392,0.125068240261613,
0.685469365367828));
#17696=CARTESIAN_POINT('Ctrl Pts',(-0.0495237900674707,0.153977456320057,
0.693411533490608));
#17697=CARTESIAN_POINT('Ctrl Pts',(-0.156243792750268,0.0418275036842162,
0.701353701613389));
#17698=CARTESIAN_POINT('Ctrl Pts',(-0.119828429739121,-0.108640739429086,
0.709295869736167));
#17699=CARTESIAN_POINT('Ctrl Pts',(0.0263620853553792,-0.159582904138124,
0.717238037858949));
#17700=CARTESIAN_POINT('Ctrl Pts',(0.148402221984423,-0.0643307340819919,
0.725180205981728));
#17701=CARTESIAN_POINT('Ctrl Pts',(0.134490677336207,0.0898549973406614,
0.733122374104509));
#17702=CARTESIAN_POINT('Ctrl Pts',(-0.00262814450422035,0.161724320044658,
0.741064542227287));
#17703=CARTESIAN_POINT('Ctrl Pts',(-0.137339315979238,0.0854375510170853,
0.749006710350069));
#17704=CARTESIAN_POINT('Ctrl Pts',(-0.146233564613262,-0.0691187920752458,
0.756948878472847));
#17705=CARTESIAN_POINT('Ctrl Pts',(-0.0211628449166461,-0.160355220783347,
0.764891046595629));
#17706=CARTESIAN_POINT('Ctrl Pts',(0.12329521486528,-0.104689793336152,
0.772833214718408));
#17707=CARTESIAN_POINT('Ctrl Pts',(0.154802191231926,0.0468822399980663,
0.780775382841188));
#17708=CARTESIAN_POINT('Ctrl Pts',(0.0444944569967772,0.155505325098544,
0.788717550963968));
#17709=CARTESIAN_POINT('Ctrl Pts',(-0.106574770936664,0.121669556739719,
0.796659719086747));
#17710=CARTESIAN_POINT('Ctrl Pts',(-0.160010559849905,-0.0236280251811701,
0.804601887209529));
#17711=CARTESIAN_POINT('Ctrl Pts',(-0.0668602374312443,-0.147279908636853,
0.812544055332307));
#17712=CARTESIAN_POINT('Ctrl Pts',(0.0875409312876049,-0.13600826514128,
0.820486223455089));
#17713=CARTESIAN_POINT('Ctrl Pts',(0.161745613525436,-0.000139078116330951,
0.828428391577867));
#17714=CARTESIAN_POINT('Ctrl Pts',(0.0877746970157421,0.135857518751215,
0.836370559700649));
#17715=CARTESIAN_POINT('Ctrl Pts',(-0.0666068593976089,0.147394671269449,
0.844312727823428));
#17716=CARTESIAN_POINT('Ctrl Pts',(-0.159969689820096,0.0239031624749592,
0.852254895946208));
#17717=CARTESIAN_POINT('Ctrl Pts',(-0.106783850056725,-0.121486098811777,
0.860197064068988));
#17718=CARTESIAN_POINT('Ctrl Pts',(0.0442269666803361,-0.155581612845794,
0.868139232191768));
#17719=CARTESIAN_POINT('Ctrl Pts',(0.154721338329289,-0.0471483860066884,
0.876081400314548));
#17720=CARTESIAN_POINT('Ctrl Pts',(0.123475068941597,0.104477606152275,
0.884023568437328));
#17721=CARTESIAN_POINT('Ctrl Pts',(-0.0208870486723946,0.160391377683462,
0.891965736560109));
#17722=CARTESIAN_POINT('Ctrl Pts',(-0.146114483894434,0.0693701696243073,
0.899907904682887));
#17723=CARTESIAN_POINT('Ctrl Pts',(-0.137486040957907,-0.0852012404790134,
0.907850072805669));
#17724=CARTESIAN_POINT('Ctrl Pts',(-0.00290626002629624,-0.161719561247554,
0.915792240928448));
#17725=CARTESIAN_POINT('Ctrl Pts',(0.134335953660838,-0.0900861498315643,
0.923734409051229));
#17726=CARTESIAN_POINT('Ctrl Pts',(0.148512632937768,0.0640754297319473,
0.931676577174007));
#17727=CARTESIAN_POINT('Ctrl Pts',(0.0266364831612253,0.159537332941991,
0.939618745296788));
#17728=CARTESIAN_POINT('Ctrl Pts',(-0.119641421660886,0.10884664928423,
0.947560913419568));
#17729=CARTESIAN_POINT('Ctrl Pts',(-0.156315493011378,-0.0415587473590326,
0.955503081542348));
#17730=CARTESIAN_POINT('Ctrl Pts',(-0.0497885138626987,-0.153892061929087,
0.963445249665127));
#17731=CARTESIAN_POINT('Ctrl Pts',(0.102349858952582,-0.125244437839883,
0.971387417787908));
#17732=CARTESIAN_POINT('Ctrl Pts',(0.160725246166783,0.018139958160622,
0.979329585910688));
#17733=CARTESIAN_POINT('Ctrl Pts',(0.0718597959603077,0.14490628889729,
0.987271754033468));
#17734=CARTESIAN_POINT('Ctrl Pts',(-0.0828366097831417,0.138923572215364,
0.995213922156248));
#17735=CARTESIAN_POINT('Ctrl Pts',(-0.161646170836971,0.00567259122332548,
1.00315609027903));
#17736=CARTESIAN_POINT('Ctrl Pts',(-0.0923712328620446,-0.132775066096718,
1.01109825840181));
#17737=CARTESIAN_POINT('Ctrl Pts',(0.0615252440718216,-0.149587122371362,
1.01904042652459));
#17738=CARTESIAN_POINT('Ctrl Pts',(0.159058276707423,-0.0293620068848675,
1.02698259464737));
#17739=CARTESIAN_POINT('Ctrl Pts',(0.1108775872014,0.117761723381742,1.03492476277015));
#17740=CARTESIAN_POINT('Ctrl Pts',(-0.0388783630684312,0.157003616909169,
1.04286693089293));
#17741=CARTESIAN_POINT('Ctrl Pts',(-0.153017738641585,0.0524140677533946,
1.05080909901571));
#17742=CARTESIAN_POINT('Ctrl Pts',(-0.126977145509477,-0.10019215216626,
1.05875126713849));
#17743=CARTESIAN_POINT('Ctrl Pts',(0.0153875577671049,-0.161012067570745,
1.06669343526127));
#17744=CARTESIAN_POINT('Ctrl Pts',(0.143655677305146,-0.0743283876822416,
1.07463560338405));
#17745=CARTESIAN_POINT('Ctrl Pts',(0.140320438123209,0.080447731368589,
1.08257777150683));
#17746=CARTESIAN_POINT('Ctrl Pts',(0.00843726195408678,0.161525463776335,
1.09051993962961));
#17747=CARTESIAN_POINT('Ctrl Pts',(-0.131175312957834,0.094629277223576,
1.09846210775239));
#17748=CARTESIAN_POINT('Ctrl Pts',(-0.150617825048456,-0.0589570489009974,
1.10640427587517));
#17749=CARTESIAN_POINT('Ctrl Pts',(-0.0320789358376135,-0.158532661344495,
1.11434644399795));
#17750=CARTESIAN_POINT('Ctrl Pts',(0.115847554194776,-0.112876069317329,
1.12228861212073));
#17751=CARTESIAN_POINT('Ctrl Pts',(0.157645783113317,0.0361865984037055,
1.13023078024351));
#17752=CARTESIAN_POINT('Ctrl Pts',(0.0550242791334153,0.152098624396442,
1.13817294836629));
#17753=CARTESIAN_POINT('Ctrl Pts',(-0.0980051173916675,0.128672684756662,
1.14611511648907));
#17754=CARTESIAN_POINT('Ctrl Pts',(-0.161251757937727,-0.0126306531673768,
1.15405728461185));
#17755=CARTESIAN_POINT('Ctrl Pts',(-0.0767752221903169,-0.142363015193798,
1.16199945273463));
#17756=CARTESIAN_POINT('Ctrl Pts',(0.0780353045016797,-0.141676229794458,
1.16994162085741));
#17757=CARTESIAN_POINT('Ctrl Pts',(0.161357475398708,-0.0111994629512984,
1.17788378898019));
#17758=CARTESIAN_POINT('Ctrl Pts',(0.0968596219472387,0.129537162519796,
1.18582595710297));
#17759=CARTESIAN_POINT('Ctrl Pts',(-0.0563715959749383,0.151604439264423,
1.19376812522575));
#17760=CARTESIAN_POINT('Ctrl Pts',(-0.157960640709981,0.0347864747270306,
1.20171029334853));
#17761=CARTESIAN_POINT('Ctrl Pts',(-0.114841510641486,-0.113899474410655,
1.20965246147131));
#17762=CARTESIAN_POINT('Ctrl Pts',(0.03348424129126,-0.158241803650584,
1.21759462959409));
#17763=CARTESIAN_POINT('Ctrl Pts',(0.151134988234409,-0.0576183839484237,
1.22553679771687));
#17764=CARTESIAN_POINT('Ctrl Pts',(0.130330559267559,0.0957893948119858,
1.23347896583965));
#17765=CARTESIAN_POINT('Ctrl Pts',(-0.0098700513554357,0.16144424710618,
1.24142113396243));
#17766=CARTESIAN_POINT('Ctrl Pts',(-0.141028680947982,0.0791995832534545,
1.24936330208521));
#17767=CARTESIAN_POINT('Ctrl Pts',(-0.142990550365238,-0.0756000353418,
1.25730547020799));
#17768=CARTESIAN_POINT('Ctrl Pts',(-0.013958385670676,-0.161142254877177,
1.26524763833077));
#17769=CARTESIAN_POINT('Ctrl Pts',(0.127861094297897,-0.0990616141723472,
1.27318980645355));
#17770=CARTESIAN_POINT('Ctrl Pts',(0.152546676219863,0.0537696421008814,
1.28113197457633));
#17771=CARTESIAN_POINT('Ctrl Pts',(0.0374838310097642,0.157342382244044,
1.28907414269911));
#17772=CARTESIAN_POINT('Ctrl Pts',(-0.111918054267102,0.116773335855419,
1.29701631082189));
#17773=CARTESIAN_POINT('Ctrl Pts',(-0.158791504053787,-0.0307720827589687,
1.30495847894467));
#17774=CARTESIAN_POINT('Ctrl Pts',(-0.060195622861772,-0.150127112226926,
1.31290064706745));
#17775=CARTESIAN_POINT('Ctrl Pts',(0.0935456330135535,-0.131950283756556,
1.32084281519023));
#17776=CARTESIAN_POINT('Ctrl Pts',(0.161589478720268,0.00710656041347678,
1.32878498331301));
#17777=CARTESIAN_POINT('Ctrl Pts',(0.0816007612396376,0.139653065139265,
1.33672715143579));
#17778=CARTESIAN_POINT('Ctrl Pts',(-0.0731426367739486,0.144263015132499,
1.34466931955857));
#17779=CARTESIAN_POINT('Ctrl Pts',(-0.160879865135934,0.0167132224867059,
1.35261148768135));
#17780=CARTESIAN_POINT('Ctrl Pts',(-0.101234609479067,-0.126147598829082,
1.36055365580413));
#17781=CARTESIAN_POINT('Ctrl Pts',(0.051151949184981,-0.153444260252591,
1.36849582392691));
#17782=CARTESIAN_POINT('Ctrl Pts',(0.15667806641111,-0.0401702148435725,
1.37643799204969));
#17783=CARTESIAN_POINT('Ctrl Pts',(0.118670980449659,0.10990387323047,1.38438016017247));
#17784=CARTESIAN_POINT('Ctrl Pts',(-0.0280509185434417,0.159294724422008,
1.39232232829525));
#17785=CARTESIAN_POINT('Ctrl Pts',(-0.149075287902345,0.0627552395607943,
1.40026449641803));
#17786=CARTESIAN_POINT('Ctrl Pts',(-0.133531390736797,-0.0912744851582948,
1.40820666454081));
#17787=CARTESIAN_POINT('Ctrl Pts',(0.00434100186018791,-0.161687417152987,
1.41614883266359));
#17788=CARTESIAN_POINT('Ctrl Pts',(0.138236546518021,-0.0839780402106489,
1.42409100078637));
#17789=CARTESIAN_POINT('Ctrl Pts',(0.145493297031458,0.07066380330362,1.43203316890915));
#17790=CARTESIAN_POINT('Ctrl Pts',(0.0194630807988606,0.160570430100525,
1.43997533703193));
#17791=CARTESIAN_POINT('Ctrl Pts',(-0.124397014000637,0.103377882332206,
1.44791750515471));
#17792=CARTESIAN_POINT('Ctrl Pts',(-0.15429723939393,-0.0485191136187331,
1.45585967327749));
#17793=CARTESIAN_POINT('Ctrl Pts',(-0.042844249846,-0.155968210152522,1.46380184140027));
#17794=CARTESIAN_POINT('Ctrl Pts',(0.107856400646442,-0.120533276677448,
1.47174400952305));
#17795=CARTESIAN_POINT('Ctrl Pts',(0.159753444358638,0.0253203827049868,
1.47968617764583));
#17796=CARTESIAN_POINT('Ctrl Pts',(0.0652924466007548,0.147982030257331,
1.48762834576861));
#17797=CARTESIAN_POINT('Ctrl Pts',(-0.0889689487809616,0.13506922671723,
1.49557051389139));
#17798=CARTESIAN_POINT('Ctrl Pts',(-0.161752593421533,-0.00156622680492735,
1.50351268201417));
#17799=CARTESIAN_POINT('Ctrl Pts',(-0.086303059730943,-0.136794666273195,
1.51145485013695));
#17800=CARTESIAN_POINT('Ctrl Pts',(0.0681115549116652,-0.14665217563879,
1.51939701825973));
#17801=CARTESIAN_POINT('Ctrl Pts',(0.160315645894948,-0.02226314405755,
1.52733918638251));
#17802=CARTESIAN_POINT('Ctrl Pts',(0.105284883301553,0.122726172858702,
1.53528135450529));
#17803=CARTESIAN_POINT('Ctrl Pts',(0.00484533846358528,0.144116573583224,
1.54057613325381));
#17804=CARTESIAN_POINT('Ctrl Pts',(-0.0388047044047284,0.131206995015745,
1.54322352262807));
#17805=CARTESIAN_POINT('Ctrl Pts',(-0.0634007094575145,0.131904027763688,
-3.88578058618805E-16));
#17806=CARTESIAN_POINT('Ctrl Pts',(-0.107282641710421,0.110811831533068,
0.00264738937425961));
#17807=CARTESIAN_POINT('Ctrl Pts',(-0.171581760589518,0.0217576868851663,
0.0079421681227796));
#17808=CARTESIAN_POINT('Ctrl Pts',(-0.111156590520044,-0.1327225175337,
0.0158843362455596));
#17809=CARTESIAN_POINT('Ctrl Pts',(0.0512451567233008,-0.165187689797298,
0.0238265043683396));
#17810=CARTESIAN_POINT('Ctrl Pts',(0.16662620135312,-0.0465387668729445,
0.0317686724911196));
#17811=CARTESIAN_POINT('Ctrl Pts',(0.129399745666171,0.114856349193662,
0.0397108406138996));
#17812=CARTESIAN_POINT('Ctrl Pts',(-0.026390801400978,0.170972456562021,
0.0476530087366796));
#17813=CARTESIAN_POINT('Ctrl Pts',(-0.157993800025737,0.070491178324729,
0.0555951768594596));
#17814=CARTESIAN_POINT('Ctrl Pts',(-0.144863967768493,-0.0945835600760224,
0.0635373449822396));
#17815=CARTESIAN_POINT('Ctrl Pts',(0.000979154756195248,-0.17300145605975,
0.0714795131050195));
#17816=CARTESIAN_POINT('Ctrl Pts',(0.145923683802689,-0.0929367665856833,
0.0794216812277997));
#17817=CARTESIAN_POINT('Ctrl Pts',(0.157187963117837,0.0722699302633024,
0.0873638493505794));
#17818=CARTESIAN_POINT('Ctrl Pts',(0.0244514793930555,0.171268692120756,
0.0953060174733598));
#17819=CARTESIAN_POINT('Ctrl Pts',(-0.130684839550095,0.113368397534175,
0.103248185596139));
#17820=CARTESIAN_POINT('Ctrl Pts',(-0.166100541844429,-0.0483893439312075,
0.11119035371892));
#17821=CARTESIAN_POINT('Ctrl Pts',(-0.0493510193195793,-0.165817291858885,
0.119132521841699));
#17822=CARTESIAN_POINT('Ctrl Pts',(0.112609073040783,-0.131339661914923,
0.12707468996448));
#17823=CARTESIAN_POINT('Ctrl Pts',(0.17140770357293,0.0234586422209967,
0.135016858087259));
#17824=CARTESIAN_POINT('Ctrl Pts',(0.0731792588499177,0.156766393306209,
0.14295902621004));
#17825=CARTESIAN_POINT('Ctrl Pts',(-0.0920889000195865,0.146460037003638,
0.150901194332819));
#17826=CARTESIAN_POINT('Ctrl Pts',(-0.172994168426659,0.00198123296575728,
0.1588433624556));
#17827=CARTESIAN_POINT('Ctrl Pts',(-0.0954190048152776,-0.144312580095855,
0.16678553057838));
#17828=CARTESIAN_POINT('Ctrl Pts',(0.0695697692503139,-0.158401246055831,
0.17472769870116));
#17829=CARTESIAN_POINT('Ctrl Pts',(0.170825487889685,-0.0273780963649298,
0.18266986682394));
#17830=CARTESIAN_POINT('Ctrl Pts',(0.115587509852263,0.128726201683253,
0.19061203494672));
#17831=CARTESIAN_POINT('Ctrl Pts',(-0.0455405018601966,0.16690407474553,
0.198554203069499));
#17832=CARTESIAN_POINT('Ctrl Pts',(-0.164948735370872,0.0521806684752238,
0.20649637119228));
#17833=CARTESIAN_POINT('Ctrl Pts',(-0.133246981425072,-0.110345590758605,
0.214438539315059));
#17834=CARTESIAN_POINT('Ctrl Pts',(0.0205226964731592,-0.171783952668295,
0.22238070743784));
#17835=CARTESIAN_POINT('Ctrl Pts',(0.155491476033395,-0.0758505658746651,
0.230322875560619));
#17836=CARTESIAN_POINT('Ctrl Pts',(0.148014089296488,0.0895697316726553,
0.2382650436834));
#17837=CARTESIAN_POINT('Ctrl Pts',(0.00494059070111224,0.172934953166096,
0.24620721180618));
#17838=CARTESIAN_POINT('Ctrl Pts',(-0.142658996543838,0.0978739912732451,
0.25414937992896));
#17839=CARTESIAN_POINT('Ctrl Pts',(-0.159568287038446,-0.0668496016012732,
0.262091548051739));
#17840=CARTESIAN_POINT('Ctrl Pts',(-0.0302966335331915,-0.170332091689456,
0.27003371617452));
#17841=CARTESIAN_POINT('Ctrl Pts',(0.126729848780061,-0.11777288690896,
0.2779758842973));
#17842=CARTESIAN_POINT('Ctrl Pts',(0.167658770158652,0.0426783815482623,
0.28591805242008));
#17843=CARTESIAN_POINT('Ctrl Pts',(0.0549950338320791,0.164031867990689,
0.293860220542859));
#17844=CARTESIAN_POINT('Ctrl Pts',(-0.108049803339193,0.135115311719503,
0.30180238866564));
#17845=CARTESIAN_POINT('Ctrl Pts',(-0.1721099202737,-0.0175807510100837,
0.309744556788419));
#17846=CARTESIAN_POINT('Ctrl Pts',(-0.0784996687135917,-0.154171039675278,
0.3176867249112));
#17847=CARTESIAN_POINT('Ctrl Pts',(0.087024343965547,-0.14952481740522,
0.325628893033979));
#17848=CARTESIAN_POINT('Ctrl Pts',(0.172825117221703,-0.00789850112384905,
0.33357106115676));
#17849=CARTESIAN_POINT('Ctrl Pts',(0.100300328103893,0.140963653630822,
0.341513229279539));
#17850=CARTESIAN_POINT('Ctrl Pts',(-0.0641098658012952,0.160688619913292,
0.349455397402319));
#17851=CARTESIAN_POINT('Ctrl Pts',(-0.16978883637574,0.033206302186043,
0.357397565525099));
#17852=CARTESIAN_POINT('Ctrl Pts',(-0.119923789760104,-0.124696399756661,
0.36533973364788));
#17853=CARTESIAN_POINT('Ctrl Pts',(0.0398037685148125,-0.168364388974385,
0.373281901770659));
#17854=CARTESIAN_POINT('Ctrl Pts',(0.163066985633654,-0.0577933011607096,
0.38122406989344));
#17855=CARTESIAN_POINT('Ctrl Pts',(0.136944091404129,0.10572238784759,0.38916623801622));
#17856=CARTESIAN_POINT('Ctrl Pts',(-0.0146336593526265,0.172385508313924,
0.397108406138999));
#17857=CARTESIAN_POINT('Ctrl Pts',(-0.152805474769431,0.0811257933285562,
0.40505057426178));
#17858=CARTESIAN_POINT('Ctrl Pts',(-0.150991776994562,-0.0844534827151793,
0.412992742384559));
#17859=CARTESIAN_POINT('Ctrl Pts',(-0.0108540995180527,-0.172664692355881,
0.42093491050734));
#17860=CARTESIAN_POINT('Ctrl Pts',(0.139227048201004,-0.102697305280782,
0.428877078630119));
#17861=CARTESIAN_POINT('Ctrl Pts',(0.16176191642983,0.0613513639265466,
0.4368192467529));
#17862=CARTESIAN_POINT('Ctrl Pts',(0.0361062507758455,0.169195880912067,
0.444761414875679));
#17863=CARTESIAN_POINT('Ctrl Pts',(-0.12262644992489,0.12203958882886,0.45270358299846));
#17864=CARTESIAN_POINT('Ctrl Pts',(-0.169020724600573,-0.0369175042249048,
0.460645751121239));
#17865=CARTESIAN_POINT('Ctrl Pts',(-0.0605746513833496,-0.162054370729346,
0.468587919244019));
#17866=CARTESIAN_POINT('Ctrl Pts',(0.103364025571403,-0.138732785167649,
0.4765300873668));
#17867=CARTESIAN_POINT('Ctrl Pts',(0.172610636112938,0.0116822841681558,
0.484472255489579));
#17868=CARTESIAN_POINT('Ctrl Pts',(0.083728171010617,0.151395181039277,
0.49241442361236));
#17869=CARTESIAN_POINT('Ctrl Pts',(-0.081857900459256,0.152414538660527,
0.500356591735139));
#17870=CARTESIAN_POINT('Ctrl Pts',(-0.172453725526818,0.0138065207282529,
0.50829875985792));
#17871=CARTESIAN_POINT('Ctrl Pts',(-0.105064221167447,-0.137449688588867,
0.516240927980699));
#17872=CARTESIAN_POINT('Ctrl Pts',(0.0585749034388466,-0.162787862415564,
0.52418309610348));
#17873=CARTESIAN_POINT('Ctrl Pts',(0.168553398866689,-0.0389956304370821,
0.532125264226259));
#17874=CARTESIAN_POINT('Ctrl Pts',(0.124119664784058,0.120520605195094,
0.54006743234904));
#17875=CARTESIAN_POINT('Ctrl Pts',(-0.0340204335384149,0.16962758491636,
0.548009600471819));
#17876=CARTESIAN_POINT('Ctrl Pts',(-0.160994319687769,0.0633382703503284,
0.5559517685946));
#17877=CARTESIAN_POINT('Ctrl Pts',(-0.14048086942825,-0.100975406844349,
0.563893936717379));
#17878=CARTESIAN_POINT('Ctrl Pts',(0.00872748937560605,-0.172785237771916,
0.57183610484016));
#17879=CARTESIAN_POINT('Ctrl Pts',(0.149940571302356,-0.0863060399984934,
0.579778272962939));
#17880=CARTESIAN_POINT('Ctrl Pts',(0.153792685935992,0.0792383569699183,
0.58772044108572));
#17881=CARTESIAN_POINT('Ctrl Pts',(0.0167549005293281,0.17219227848818,
0.595662609208499));
#17882=CARTESIAN_POINT('Ctrl Pts',(-0.135632095058532,0.107400382926376,
0.60360477733128));
#17883=CARTESIAN_POINT('Ctrl Pts',(-0.163766157558233,-0.0557812970565469,
0.611546945454059));
#17884=CARTESIAN_POINT('Ctrl Pts',(-0.0418735953979919,-0.167861578305293,
0.61948911357684));
#17885=CARTESIAN_POINT('Ctrl Pts',(0.118379481984711,-0.126163408751231,
0.627431281699619));
#17886=CARTESIAN_POINT('Ctrl Pts',(0.17018479228316,0.0311134044783985,
0.6353734498224));
#17887=CARTESIAN_POINT('Ctrl Pts',(0.0660833491022344,0.159887142804326,
0.643315617945179));
#17888=CARTESIAN_POINT('Ctrl Pts',(-0.0985572308567358,0.142187832491218,
0.651257786067961));
#17889=CARTESIAN_POINT('Ctrl Pts',(-0.172909262181909,-0.00577013989488307,
0.659199954190738));
#17890=CARTESIAN_POINT('Ctrl Pts',(-0.0888586457050277,-0.148442071348278,
0.667142122313521));
#17891=CARTESIAN_POINT('Ctrl Pts',(0.0765956190331784,-0.155125815413241,
0.675084290436298));
#17892=CARTESIAN_POINT('Ctrl Pts',(0.171880427770071,-0.0196983758791502,
0.683026458559081));
#17893=CARTESIAN_POINT('Ctrl Pts',(0.109705106722326,0.133774799651286,
0.690968626681858));
#17894=CARTESIAN_POINT('Ctrl Pts',(-0.0529713625168984,0.164696515493808,
0.698910794804641));
#17895=CARTESIAN_POINT('Ctrl Pts',(-0.167120621735807,0.0447393032280997,
0.706852962927418));
#17896=CARTESIAN_POINT('Ctrl Pts',(-0.12817022249092,-0.116203707037801,
0.7147951310502));
#17897=CARTESIAN_POINT('Ctrl Pts',(0.0281972679828983,-0.17069218359667,
0.722737299172979));
#17898=CARTESIAN_POINT('Ctrl Pts',(0.158733164168978,-0.0688090841067,0.73067946729576));
#17899=CARTESIAN_POINT('Ctrl Pts',(0.14385317469873,0.0961102054508026,
0.738621635418538));
#17900=CARTESIAN_POINT('Ctrl Pts',(-0.00281110139369983,0.172982673038814,
0.746563803541321));
#17901=CARTESIAN_POINT('Ctrl Pts',(-0.146900119814081,0.0913852409380608,
0.754505971664098));
#17902=CARTESIAN_POINT('Ctrl Pts',(-0.156413536862055,-0.0739304602244656,
0.762448139786881));
#17903=CARTESIAN_POINT('Ctrl Pts',(-0.0226360851712103,-0.171518264656626,
0.770390307909658));
#17904=CARTESIAN_POINT('Ctrl Pts',(0.131878346029848,-0.111977717922496,
0.778332476032441));
#17905=CARTESIAN_POINT('Ctrl Pts',(0.165578663890314,0.0501459223366878,
0.786274644155218));
#17906=CARTESIAN_POINT('Ctrl Pts',(0.047591915084802,0.166330746049129,
0.794216812278001));
#17907=CARTESIAN_POINT('Ctrl Pts',(-0.113993917241593,0.130139518573781,
0.802158980400778));
#17908=CARTESIAN_POINT('Ctrl Pts',(-0.171149610334614,-0.0252728776558711,
0.81010114852356));
#17909=CARTESIAN_POINT('Ctrl Pts',(-0.0715146774936035,-0.157532721571376,
0.818043316646339));
#17910=CARTESIAN_POINT('Ctrl Pts',(0.0936350469135118,-0.14547640857611,
0.825985484769119));
#17911=CARTESIAN_POINT('Ctrl Pts',(0.173005448853992,-0.000148759965830227,
0.8339276528919));
#17912=CARTESIAN_POINT('Ctrl Pts',(0.0938850861191564,0.145315168055841,
0.841869821014678));
#17913=CARTESIAN_POINT('Ctrl Pts',(-0.0712436606821878,0.157655473343934,
0.849811989137461));
#17914=CARTESIAN_POINT('Ctrl Pts',(-0.171105895159299,0.0255671684868261,
0.857754157260238));
#17915=CARTESIAN_POINT('Ctrl Pts',(-0.114217551294,-0.129943289319231,0.86569632538302));
#17916=CARTESIAN_POINT('Ctrl Pts',(0.0473058035714782,-0.166412344527548,
0.873638493505798));
#17917=CARTESIAN_POINT('Ctrl Pts',(0.16549218245563,-0.0504305959589149,
0.88158066162858));
#17918=CARTESIAN_POINT('Ctrl Pts',(0.132070720552549,0.111750759440056,
0.889522829751358));
#17919=CARTESIAN_POINT('Ctrl Pts',(-0.022341089517305,0.171556938600217,
0.89746499787414));
#17920=CARTESIAN_POINT('Ctrl Pts',(-0.156286166401977,0.074199337288632,
0.905407165996919));
#17921=CARTESIAN_POINT('Ctrl Pts',(-0.147057058974526,-0.0911324797668838,
0.913349334119699));
#17922=CARTESIAN_POINT('Ctrl Pts',(-0.00310857778072832,-0.172977582960567,
0.92129150224248));
#17923=CARTESIAN_POINT('Ctrl Pts',(0.143687680016546,-0.0963574495000853,
0.929233670365259));
#17924=CARTESIAN_POINT('Ctrl Pts',(0.158851261322436,0.0685360068793772,
0.93717583848804));
#17925=CARTESIAN_POINT('Ctrl Pts',(0.0284907678468484,0.170643439985825,
0.945118006610819));
#17926=CARTESIAN_POINT('Ctrl Pts',(-0.127970195944242,0.116423951198588,
0.9530601747336));
#17927=CARTESIAN_POINT('Ctrl Pts',(-0.167197313372666,-0.0444518375735043,
0.961002342856378));
#17928=CARTESIAN_POINT('Ctrl Pts',(-0.0532545149190986,-0.164605176417482,
0.96894451097916));
#17929=CARTESIAN_POINT('Ctrl Pts',(0.10947489024455,-0.133963263130763,
0.976886679101939));
#17930=CARTESIAN_POINT('Ctrl Pts',(0.1719140491614,0.0194027617526574,0.984828847224719));
#17931=CARTESIAN_POINT('Ctrl Pts',(0.0768622776450996,0.154993863549195,
0.992771015347499));
#17932=CARTESIAN_POINT('Ctrl Pts',(-0.088603236555915,0.148594663210074,
1.00071318347028));
#17933=CARTESIAN_POINT('Ctrl Pts',(-0.172899083515371,0.00606748566075909,
1.00865535159306));
#17934=CARTESIAN_POINT('Ctrl Pts',(-0.0988016073770141,-0.142018132090297,
1.01659751971584));
#17935=CARTESIAN_POINT('Ctrl Pts',(0.0658082913934689,-0.160000550769587,
1.02453968783862));
#17936=CARTESIAN_POINT('Ctrl Pts',(0.170131034504888,-0.0314060274628177,
1.0324818559614));
#17937=CARTESIAN_POINT('Ctrl Pts',(0.118596271784576,0.125959643463681,
1.04042402408418));
#17938=CARTESIAN_POINT('Ctrl Pts',(-0.0415848597483297,0.167933340651612,
1.04836619220696));
#17939=CARTESIAN_POINT('Ctrl Pts',(-0.163669987576804,0.0560628453550813,
1.05630836032974));
#17940=CARTESIAN_POINT('Ctrl Pts',(-0.135816592328243,-0.107166975841641,
1.06425052845252));
#17941=CARTESIAN_POINT('Ctrl Pts',(0.0164587544616562,-0.172220837485682,
1.0721926965753));
#17942=CARTESIAN_POINT('Ctrl Pts',(0.153656191292587,-0.0795027190739688,
1.08013486469808));
#17943=CARTESIAN_POINT('Ctrl Pts',(0.150088771199207,0.0860480576341552,
1.08807703282086));
#17944=CARTESIAN_POINT('Ctrl Pts',(0.00902461748204118,0.172769973496559,
1.09601920094364));
#17945=CARTESIAN_POINT('Ctrl Pts',(-0.140307012982855,0.101216844302358,
1.10396136906642));
#17946=CARTESIAN_POINT('Ctrl Pts',(-0.161103005268346,-0.0630613126743013,
1.1119035371892));
#17947=CARTESIAN_POINT('Ctrl Pts',(-0.0343120939874615,-0.1695688287065,
1.11984570531198));
#17948=CARTESIAN_POINT('Ctrl Pts',(0.123912220401285,-0.120733877175888,
1.12778787343476));
#17949=CARTESIAN_POINT('Ctrl Pts',(0.168620210916381,0.0387057093103061,
1.13573004155754));
#17950=CARTESIAN_POINT('Ctrl Pts',(0.0588547652196237,0.162686889679659,
1.14367220968032));
#17951=CARTESIAN_POINT('Ctrl Pts',(-0.104827691798069,0.137630165643247,
1.1516143778031));
#17952=CARTESIAN_POINT('Ctrl Pts',(-0.172477213770776,-0.0135099294065116,
1.15955654592588));
#17953=CARTESIAN_POINT('Ctrl Pts',(-0.0821198886720452,-0.152273541192125,
1.16749871404866));
#17954=CARTESIAN_POINT('Ctrl Pts',(0.083467690946984,-0.15153894559049,
1.17544088217144));
#17955=CARTESIAN_POINT('Ctrl Pts',(0.172590290696882,-0.0119791076405788,
1.18338305029422));
#17956=CARTESIAN_POINT('Ctrl Pts',(0.103602453294194,0.13855482356859,1.191325218417));
#17957=CARTESIAN_POINT('Ctrl Pts',(-0.0602958748103966,0.162158302111078,
1.19926738653978));
#17958=CARTESIAN_POINT('Ctrl Pts',(-0.168956987158091,0.0372081167644847,
1.20720955466256));
#17959=CARTESIAN_POINT('Ctrl Pts',(-0.122836141658186,-0.121828526073448,
1.21515172278534));
#17960=CARTESIAN_POINT('Ctrl Pts',(0.0358152290369173,-0.169257723108079,
1.22309389090812));
#17961=CARTESIAN_POINT('Ctrl Pts',(0.161656170495932,-0.0616294572691503,
1.2310360590309));
#17962=CARTESIAN_POINT('Ctrl Pts',(0.13940345221127,0.102457722863032,1.23897822715368));
#17963=CARTESIAN_POINT('Ctrl Pts',(-0.0105571497596809,0.172683102970871,
1.24692039527646));
#17964=CARTESIAN_POINT('Ctrl Pts',(-0.150846317973597,0.0847130203482025,
1.25486256339924));
#17965=CARTESIAN_POINT('Ctrl Pts',(-0.152944761892581,-0.0808628918127005,
1.26280473152202));
#17966=CARTESIAN_POINT('Ctrl Pts',(-0.0149300913057054,-0.172360087712588,
1.2707468996448));
#17967=CARTESIAN_POINT('Ctrl Pts',(0.136762076743997,-0.105957736043287,
1.27868906776758));
#17968=CARTESIAN_POINT('Ctrl Pts',(0.163166132393764,0.0575127872937276,
1.28663123589036));
#17969=CARTESIAN_POINT('Ctrl Pts',(0.0400932480780463,0.168295688956082,
1.29457340401314));
#17970=CARTESIAN_POINT('Ctrl Pts',(-0.119709170414695,0.124902449862528,
1.30251557213592));
#17971=CARTESIAN_POINT('Ctrl Pts',(-0.169845690614082,-0.0329142650230248,
1.3104577402587));
#17972=CARTESIAN_POINT('Ctrl Pts',(-0.0643861093061943,-0.160578131733314,
1.31839990838148));
#17973=CARTESIAN_POINT('Ctrl Pts',(0.100057762773863,-0.141135932963798,
1.32634207650426));
#17974=CARTESIAN_POINT('Ctrl Pts',(0.172838444806952,0.00760127985757451,
1.33428424462704));
#17975=CARTESIAN_POINT('Ctrl Pts',(0.0872813550697656,0.149374939398002,
1.34222641274982));
#17976=CARTESIAN_POINT('Ctrl Pts',(-0.0782344227434143,0.154305808621531,
1.3501685808726));
#17977=CARTESIAN_POINT('Ctrl Pts',(-0.172079431848303,0.0178767046294837,
1.35811074899538));
#17978=CARTESIAN_POINT('Ctrl Pts',(-0.108282003268856,-0.134929297194493,
1.36605291711816));
#17979=CARTESIAN_POINT('Ctrl Pts',(0.0547128650701426,-0.164126201264144,
1.37399508524094));
#17980=CARTESIAN_POINT('Ctrl Pts',(0.167585127127835,-0.0429666431014547,
1.38193725336372));
#17981=CARTESIAN_POINT('Ctrl Pts',(0.126932197981417,0.117554773230619,
1.3898794214865));
#17982=CARTESIAN_POINT('Ctrl Pts',(-0.0300036684000219,0.170383942402052,
1.39782158960928));
#17983=CARTESIAN_POINT('Ctrl Pts',(-0.159453085214751,0.0671239123677834,
1.40576375773206));
#17984=CARTESIAN_POINT('Ctrl Pts',(-0.142827107870127,-0.0976285101620078,
1.41370592585484));
#17985=CARTESIAN_POINT('Ctrl Pts',(0.00464319840846943,-0.172943201171859,
1.42164809397762));
#17986=CARTESIAN_POINT('Ctrl Pts',(0.147859810582222,-0.0898241270588577,
1.4295902621004));
#17987=CARTESIAN_POINT('Ctrl Pts',(0.155621735944117,0.0755830265922534,
1.43753243022318));
#17988=CARTESIAN_POINT('Ctrl Pts',(0.0208179928734729,0.171748455656582,
1.44547459834596));
#17989=CARTESIAN_POINT('Ctrl Pts',(-0.133056846329205,0.11057447892796,
1.45341676646874));
#17990=CARTESIAN_POINT('Ctrl Pts',(-0.165038560097216,-0.0518967460486161,
1.46135893459152));
#17991=CARTESIAN_POINT('Ctrl Pts',(-0.0458268296361176,-0.166825854601292,
1.4693011027143));
#17992=CARTESIAN_POINT('Ctrl Pts',(0.115364766925686,-0.128924136976022,
1.47724327083708));
#17993=CARTESIAN_POINT('Ctrl Pts',(0.170874595884426,0.0270830477535184,
1.48518543895986));
#17994=CARTESIAN_POINT('Ctrl Pts',(0.0698377457337486,0.158283721017069,
1.49312760708264));
#17995=CARTESIAN_POINT('Ctrl Pts',(-0.0951624750893037,0.144471999488883,
1.50106977520542));
#17996=CARTESIAN_POINT('Ctrl Pts',(-0.173012914651864,-0.00167525885548286,
1.5090119433282));
#17997=CARTESIAN_POINT('Ctrl Pts',(-0.092311001583214,-0.14631755460685,
1.51695411145098));
#17998=CARTESIAN_POINT('Ctrl Pts',(0.072853104778531,-0.156861289272697,
1.52489627957376));
#17999=CARTESIAN_POINT('Ctrl Pts',(0.171475934783304,-0.0238129810547936,
1.53283844769654));
#18000=CARTESIAN_POINT('Ctrl Pts',(0.11261423476106,0.131269690464983,1.54078061581932));
#18001=CARTESIAN_POINT('Ctrl Pts',(0.00518264413773371,0.154149172621267,
1.54607539456784));
#18002=CARTESIAN_POINT('Ctrl Pts',(-0.0415060733757155,0.140340900570467,
1.5487227839421));
#18003=CARTESIAN_POINT('Ctrl Pts',(-0.146248097568756,-0.000123763188177425,
1.45893449541571));
#18004=CARTESIAN_POINT('Ctrl Pts',(-0.146367493381718,-0.0150081347743067,
1.45974264180765));
#18005=CARTESIAN_POINT('Ctrl Pts',(-0.144277648885518,-0.0298597803798721,
1.46055078819958));
#18006=CARTESIAN_POINT('Ctrl Pts',(-0.139839652725699,-0.043973059977961,
1.46135893459152));
#18007=CARTESIAN_POINT('Ctrl Pts',(-0.125301316610186,-0.0902064488995044,
1.46400632396578));
#18008=CARTESIAN_POINT('Ctrl Pts',(-0.08556407312315,-0.1285161517504,1.46665371334004));
#18009=CARTESIAN_POINT('Ctrl Pts',(-0.0388301852859989,-0.141354050238301,
1.4693011027143));
#18010=CARTESIAN_POINT('Ctrl Pts',(0.00790370255115092,-0.154191948726202,
1.47194849208856));
#18011=CARTESIAN_POINT('Ctrl Pts',(0.0616342347384179,-0.141558042851112,
1.47459588146282));
#18012=CARTESIAN_POINT('Ctrl Pts',(0.0977511389918415,-0.109239892458645,
1.47724327083708));
#18013=CARTESIAN_POINT('Ctrl Pts',(0.133868043245265,-0.0769217420661769,
1.47989066021134));
#18014=CARTESIAN_POINT('Ctrl Pts',(0.152371319564846,-0.024919347156331,
1.4825380495856));
#18015=CARTESIAN_POINT('Ctrl Pts',(0.144783482699524,0.0229486291758506,
1.48518543895986));
#18016=CARTESIAN_POINT('Ctrl Pts',(0.137195645834202,0.0708166055080336,
1.48783282833412));
#18017=CARTESIAN_POINT('Ctrl Pts',(0.103516695783975,0.114550163262552,
1.49048021770838));
#18018=CARTESIAN_POINT('Ctrl Pts',(0.0591771839550196,0.13411498855178,
1.49312760708264));
#18019=CARTESIAN_POINT('Ctrl Pts',(0.014837672126065,0.153679813841007,
1.4957749964569));
#18020=CARTESIAN_POINT('Ctrl Pts',(-0.0401624014816186,0.149075906664945,
1.49842238583116));
#18021=CARTESIAN_POINT('Ctrl Pts',(-0.0806375115458872,0.122416076686187,
1.50106977520542));
#18022=CARTESIAN_POINT('Ctrl Pts',(-0.0937869288003098,0.113754921033589,
1.50192985013695));
#18023=CARTESIAN_POINT('Ctrl Pts',(-0.105403311347291,0.102765876910903,
1.50278992506847));
#18024=CARTESIAN_POINT('Ctrl Pts',(-0.115078604842433,0.0902138214954038,
1.50365));
#18025=CARTESIAN_POINT('Ctrl Pts',(-0.0686146973663081,-0.0959584553529135,
1.07336015076065E-17));
#18026=CARTESIAN_POINT('Ctrl Pts',(-0.0712979561985307,-0.0944995001033786,
9.02613639135873E-18));
#18027=CARTESIAN_POINT('Ctrl Pts',(-0.0739152333025289,-0.0929325179580126,
1.64107321374712E-17));
#18028=CARTESIAN_POINT('Ctrl Pts',(-0.0764591723283171,-0.0912589988675934,
1.6154612370034E-17));
#18029=CARTESIAN_POINT('Ctrl Pts',(-0.0824897891353913,-0.0872917841461184,
1.52077426268717E-17));
#18030=CARTESIAN_POINT('Ctrl Pts',(-0.0881090519769445,-0.0827275518978924,
1.30971627060498E-17));
#18031=CARTESIAN_POINT('Ctrl Pts',(-0.0932912133381108,-0.0776621329443405,
1.43114686768087E-17));
#18032=CARTESIAN_POINT('Ctrl Pts',(-0.0960634919631888,-0.074952307504085,
1.49610807310118E-17));
#18033=CARTESIAN_POINT('Ctrl Pts',(-0.0987043519497191,-0.0721043812799658,
1.74993329480528E-17));
#18034=CARTESIAN_POINT('Ctrl Pts',(-0.101206237074718,-0.0691378820326018,
9.97465998686664E-18));
#18035=CARTESIAN_POINT('Ctrl Pts',(-0.105823426721714,-0.0636632543305198,
-3.91200561030858E-18));
#18036=CARTESIAN_POINT('Ctrl Pts',(-0.109972666997065,-0.0577811896139199,
2.24798207762934E-18));
#18037=CARTESIAN_POINT('Ctrl Pts',(-0.113625452403263,-0.0515741981665521,
9.54097911787244E-18));
#18038=CARTESIAN_POINT('Ctrl Pts',(-0.115386295340069,-0.0485820878086944,
1.30566037435822E-17));
#18039=CARTESIAN_POINT('Ctrl Pts',(-0.117027309103105,-0.0455212415157476,
-2.79521757168051E-18));
#18040=CARTESIAN_POINT('Ctrl Pts',(-0.118543833519887,-0.0424058589801268,
-3.46944695195361E-18));
#18041=CARTESIAN_POINT('Ctrl Pts',(-0.122700941917732,-0.0338659484069709,
-5.31764971597768E-18));
#18042=CARTESIAN_POINT('Ctrl Pts',(-0.125931492798984,-0.0249085743588085,
-1.15219401683824E-18));
#18043=CARTESIAN_POINT('Ctrl Pts',(-0.128167520083254,-0.0157105262534848,
9.54097911787244E-18));
#18044=CARTESIAN_POINT('Ctrl Pts',(-0.128992166906242,-0.0123182862745252,
1.3484621181291E-17));
#18045=CARTESIAN_POINT('Ctrl Pts',(-0.129681150280034,-0.00889298553317688,
1.10989611676181E-17));
#18046=CARTESIAN_POINT('Ctrl Pts',(-0.130229483957028,-0.00544263935519351,
9.54097911787244E-18));
#18047=CARTESIAN_POINT('Ctrl Pts',(-0.130761899349706,-0.00209245771889707,
8.02822573502553E-18));
#18048=CARTESIAN_POINT('Ctrl Pts',(-0.131160261982709,0.00127366115726457,
1.11791151702242E-17));
#18049=CARTESIAN_POINT('Ctrl Pts',(-0.131420990891747,0.00464012593483382,
8.67361737988404E-18));
#18050=CARTESIAN_POINT('Ctrl Pts',(-0.131728666658755,0.00861275649723166,
5.71697955546795E-18));
#18051=CARTESIAN_POINT('Ctrl Pts',(-0.131845259942619,0.0125891451047215,
-9.26473565962443E-18));
#18052=CARTESIAN_POINT('Ctrl Pts',(-0.131765781147177,0.0165567997877194,
-1.04083408558608E-17));
#18053=CARTESIAN_POINT('Ctrl Pts',(-0.131635692412819,0.0230509492424239,
-1.21888544026837E-17));
#18054=CARTESIAN_POINT('Ctrl Pts',(-0.13098103789945,0.0295216962360144,
-2.67049856555875E-17));
#18055=CARTESIAN_POINT('Ctrl Pts',(-0.129839098367345,0.0359278479980343,
-3.46944695195361E-17));
#18056=CARTESIAN_POINT('Ctrl Pts',(-0.129254890951344,0.0392051855997028,
-3.87818275556788E-17));
#18057=CARTESIAN_POINT('Ctrl Pts',(-0.128542951403208,0.0424656461998481,
-3.10678831811161E-17));
#18058=CARTESIAN_POINT('Ctrl Pts',(-0.1277070993652,0.0457037274559979,
-3.29597460435593E-17));
#18059=CARTESIAN_POINT('Ctrl Pts',(-0.126886363095037,0.0488832504000222,
-3.48173959609792E-17));
#18060=CARTESIAN_POINT('Ctrl Pts',(-0.125948031872817,0.0520333657183593,
-3.53366201082739E-17));
#18061=CARTESIAN_POINT('Ctrl Pts',(-0.124899042599898,0.0551436241923499,
-3.46944695195361E-17));
#18062=CARTESIAN_POINT('Ctrl Pts',(-0.122234979928128,0.0630425834229368,
-3.30636335736642E-17));
#18063=CARTESIAN_POINT('Ctrl Pts',(-0.118856305871375,0.070695441500891,
-2.1366080483524E-17));
#18064=CARTESIAN_POINT('Ctrl Pts',(-0.114834854776346,0.078019637496205,
-1.73472347597681E-17));
#18065=CARTESIAN_POINT('Ctrl Pts',(-0.11215901866562,0.0828930893082948,
-1.46731322388254E-17));
#18066=CARTESIAN_POINT('Ctrl Pts',(-0.109198005187061,0.0876211033078822,
8.28606628989234E-18));
#18067=CARTESIAN_POINT('Ctrl Pts',(-0.105966883726074,0.0921780034666525,
8.67361737988404E-18));
#18068=CARTESIAN_POINT('Ctrl Pts',(-0.104137243112614,0.094758373688769,
8.89307035390601E-18));
#18069=CARTESIAN_POINT('Ctrl Pts',(-0.102221042121924,0.0972831505018574,
-2.31209379389524E-17));
#18070=CARTESIAN_POINT('Ctrl Pts',(-0.100229777791505,0.0997373632832089,
-2.08166817117217E-17));
#18071=CARTESIAN_POINT('Ctrl Pts',(-0.0937202782075859,0.107760254486057,
-1.32840027382311E-17));
#18072=CARTESIAN_POINT('Ctrl Pts',(-0.0863914655699752,0.115060936709644,
5.4842312373535E-18));
#18073=CARTESIAN_POINT('Ctrl Pts',(-0.0783508402622743,0.121487309774744,
1.38777878078145E-17));
#18074=CARTESIAN_POINT('Ctrl Pts',(-0.073610711791116,0.125275800441382,
1.8825977152717E-17));
#18075=CARTESIAN_POINT('Ctrl Pts',(-0.068622257850438,0.128760167547443,
-9.09579695168528E-18));
#18076=CARTESIAN_POINT('Ctrl Pts',(-0.0634007094575209,0.131904027763685,
-6.93889390390723E-18));
#18077=CARTESIAN_POINT('Origin',(0.,0.,0.));
#18078=CARTESIAN_POINT('Origin',(-0.0721687836487033,-0.125,-0.3));
#18079=CARTESIAN_POINT('',(-0.0721687836487033,-0.125,-0.3));
#18080=CARTESIAN_POINT('',(0.0721687836487032,-0.125,-0.3));
#18081=CARTESIAN_POINT('',(-0.0360843918243517,-0.125,-0.3));
#18082=CARTESIAN_POINT('',(-0.0721687836487033,-0.125,-0.15));
#18083=CARTESIAN_POINT('',(-0.0721687836487033,-0.125,-0.3));
#18084=CARTESIAN_POINT('',(0.0721687836487032,-0.125,-0.15));
#18085=CARTESIAN_POINT('',(-0.0721687836487033,-0.125,-0.15));
#18086=CARTESIAN_POINT('',(0.0721687836487032,-0.125,-0.3));
#18087=CARTESIAN_POINT('Origin',(-0.144337567297406,1.76762539787485E-17,
-0.3));
#18088=CARTESIAN_POINT('',(-0.144337567297406,1.76762539787485E-17,-0.3));
#18089=CARTESIAN_POINT('',(-0.126295371385231,-0.03125,-0.3));
#18090=CARTESIAN_POINT('',(-0.144337567297406,2.77555756156289E-17,-0.15));
#18091=CARTESIAN_POINT('',(-0.144337567297406,1.76762539787485E-17,-0.3));
#18092=CARTESIAN_POINT('',(-0.144337567297406,1.76762539787485E-17,-0.15));
#18093=CARTESIAN_POINT('Origin',(-0.0721687836487032,0.125,-0.3));
#18094=CARTESIAN_POINT('',(-0.0721687836487032,0.125,-0.3));
#18095=CARTESIAN_POINT('',(-0.090210979560879,0.09375,-0.3));
#18096=CARTESIAN_POINT('',(-0.0721687836487032,0.125,-0.15));
#18097=CARTESIAN_POINT('',(-0.0721687836487032,0.125,-0.3));
#18098=CARTESIAN_POINT('',(-0.0721687836487032,0.125,-0.15));
#18099=CARTESIAN_POINT('Origin',(0.0721687836487032,0.125,-0.3));
#18100=CARTESIAN_POINT('',(0.0721687836487032,0.125,-0.3));
#18101=CARTESIAN_POINT('',(0.0360843918243516,0.125,-0.3));
#18102=CARTESIAN_POINT('',(0.0721687836487032,0.125,-0.15));
#18103=CARTESIAN_POINT('',(0.0721687836487032,0.125,-0.3));
#18104=CARTESIAN_POINT('',(0.0721687836487032,0.125,-0.15));
#18105=CARTESIAN_POINT('Origin',(0.144337567297406,0.,-0.3));
#18106=CARTESIAN_POINT('',(0.144337567297406,0.,-0.3));
#18107=CARTESIAN_POINT('',(0.126295371385231,0.03125,-0.3));
#18108=CARTESIAN_POINT('',(0.144337567297406,0.,-0.15));
#18109=CARTESIAN_POINT('',(0.144337567297406,0.,-0.3));
#18110=CARTESIAN_POINT('',(0.144337567297406,0.,-0.15));
#18111=CARTESIAN_POINT('Origin',(0.0721687836487032,-0.125,-0.3));
#18112=CARTESIAN_POINT('',(0.0902109795608791,-0.09375,-0.3));
#18113=CARTESIAN_POINT('',(0.0721687836487032,-0.125,-0.15));
#18114=CARTESIAN_POINT('Origin',(0.,0.,-0.15));
#18115=CARTESIAN_POINT('Origin',(0.,0.,0.));
#18116=CARTESIAN_POINT('',(-0.275,-3.36777869765522E-17,0.));
#18117=CARTESIAN_POINT('Origin',(0.,0.,0.));
#18118=CARTESIAN_POINT('Origin',(0.,0.,-0.3));
#18119=CARTESIAN_POINT('',(-0.275,-3.36777869765522E-17,-0.3));
#18120=CARTESIAN_POINT('',(-0.275,-3.36777869765522E-17,-0.3));
#18121=CARTESIAN_POINT('Origin',(0.,0.,-0.3));
#18122=CARTESIAN_POINT('Origin',(0.,0.,-0.3));
#18123=CARTESIAN_POINT('Origin',(0.,0.,1.6));
#18124=CARTESIAN_POINT('',(0.,0.,0.));
#18125=CARTESIAN_POINT('Origin',(0.,0.,0.12));
#18126=CARTESIAN_POINT('',(-0.12639138516214,8.91322620741042E-5,0.00934196736194174));
#18127=CARTESIAN_POINT('',(-0.12645,1.54856587752183E-17,-5.55111512312578E-17));
#18128=CARTESIAN_POINT('',(-0.12645,1.54856587752183E-17,0.12));
#18129=CARTESIAN_POINT('',(-0.0488748409397564,0.116622692573588,0.));
#18130=CARTESIAN_POINT('Origin',(0.,0.,0.));
#18131=CARTESIAN_POINT('Ctrl Pts',(-0.0489111879062984,0.116810626195002,
1.20007714660797E-17));
#18132=CARTESIAN_POINT('Ctrl Pts',(-0.0838963038512042,0.101957324585112,
0.00240024091002088));
#18133=CARTESIAN_POINT('Ctrl Pts',(-0.11198221847721,0.0702793053867637,
0.00480048182004174));
#18134=CARTESIAN_POINT('Ctrl Pts',(-0.122072221370749,0.0336561163696377,
0.00720072273006261));
#18135=CARTESIAN_POINT('Ctrl Pts',(-0.125072637487486,0.022765653033531,
0.00791447094068899));
#18136=CARTESIAN_POINT('Ctrl Pts',(-0.126481745582665,0.0114379076904012,
0.00862821915131536));
#18137=CARTESIAN_POINT('Ctrl Pts',(-0.12639138516214,8.91322620741042E-5,
0.00934196736194174));
#18138=CARTESIAN_POINT('Origin',(0.,0.,0.12));
#18139=CARTESIAN_POINT('',(-0.126396145829628,-9.95859796292312E-5,0.0593419673619417));
#18140=CARTESIAN_POINT('',(-0.126575671592806,-7.20628672610732E-5,0.0456580326380584));
#18141=CARTESIAN_POINT('',(-0.12645,1.54856587752183E-17,0.12));
#18142=CARTESIAN_POINT('',(-0.10808967569503,-0.0656218295092665,0.));
#18143=CARTESIAN_POINT('Ctrl Pts',(-0.126575671592806,-7.20628672610732E-5,
0.0456580326380584));
#18144=CARTESIAN_POINT('Ctrl Pts',(-0.126327459688109,0.0361497101693465,
0.0433719816070355));
#18145=CARTESIAN_POINT('Ctrl Pts',(-0.109912066394173,0.0725710138228805,
0.0410859305760125));
#18146=CARTESIAN_POINT('Ctrl Pts',(-0.0824515099939393,0.0961223418729112,
0.0387998795449896));
#18147=CARTESIAN_POINT('Ctrl Pts',(-0.05137998778939,0.122770586059505,
0.036213220908657));
#18148=CARTESIAN_POINT('Ctrl Pts',(-0.00616751748104999,0.132941603485868,
0.0336265622723243));
#18149=CARTESIAN_POINT('Ctrl Pts',(0.0333172074018229,0.122176268745047,
0.0310399036359917));
#18150=CARTESIAN_POINT('Ctrl Pts',(0.0728019322846963,0.111410934004226,
0.028453244999659));
#18151=CARTESIAN_POINT('Ctrl Pts',(0.106558911742102,0.0797092470962188,
0.0258665863633264));
#18152=CARTESIAN_POINT('Ctrl Pts',(0.11981357554495,0.0409763259700822,
0.0232799277269937));
#18153=CARTESIAN_POINT('Ctrl Pts',(0.133068239347797,0.00224340484394604,
0.0206932690906611));
#18154=CARTESIAN_POINT('Ctrl Pts',(0.125820587496086,-0.0435207505003201,
0.0181066104543285));
#18155=CARTESIAN_POINT('Ctrl Pts',(0.101166903546451,-0.0762076816581678,
0.0155199518179958));
#18156=CARTESIAN_POINT('Ctrl Pts',(0.0765132195968157,-0.108894612816016,
0.0129332931816632));
#18157=CARTESIAN_POINT('Ctrl Pts',(0.0344535035492562,-0.128504319787445,
0.0103466345453306));
#18158=CARTESIAN_POINT('Ctrl Pts',(-0.00636464094143544,-0.126469737202777,
0.00775997590899791));
#18159=CARTESIAN_POINT('Ctrl Pts',(-0.0471827854321269,-0.124435154618108,
0.00517331727266527));
#18160=CARTESIAN_POINT('Ctrl Pts',(-0.0867593583659505,-0.100756282477341,
0.00258665863633259));
#18161=CARTESIAN_POINT('Ctrl Pts',(-0.108089675695031,-0.0656218295092657,
-5.55111512312578E-17));
#18162=CARTESIAN_POINT('Origin',(0.,0.,0.));
#18163=CARTESIAN_POINT('Ctrl Pts',(-0.12639138516214,8.91322620741042E-5,
0.00934196736194174));
#18164=CARTESIAN_POINT('Ctrl Pts',(-0.126154274972366,-0.0296906128949183,
0.011214877787648));
#18165=CARTESIAN_POINT('Ctrl Pts',(-0.115592373032178,-0.0596151635265703,
0.0130877882133543));
#18166=CARTESIAN_POINT('Ctrl Pts',(-0.0963650578556872,-0.0821635787359664,
0.0149606986390606));
#18167=CARTESIAN_POINT('Ctrl Pts',(-0.0698103971670931,-0.113304978845907,
0.0175473572753932));
#18168=CARTESIAN_POINT('Ctrl Pts',(-0.0267272342632827,-0.130377059081323,
0.0201340159117258));
#18169=CARTESIAN_POINT('Ctrl Pts',(0.0139574509341311,-0.125868770046104,
0.0227206745480584));
#18170=CARTESIAN_POINT('Ctrl Pts',(0.0546421361315456,-0.121360481010885,
0.0253073331843911));
#18171=CARTESIAN_POINT('Ctrl Pts',(0.0929283436225635,-0.0952718227050311,
0.0278939918207237));
#18172=CARTESIAN_POINT('Ctrl Pts',(0.112018291148455,-0.0590635258734944,
0.0304806504570564));
#18173=CARTESIAN_POINT('Ctrl Pts',(0.131108238674346,-0.0228552290419586,
0.033067309093389));
#18174=CARTESIAN_POINT('Ctrl Pts',(0.131001926235112,0.0234727063152593,
0.0356539677297216));
#18175=CARTESIAN_POINT('Ctrl Pts',(0.111741771403992,0.0595891814911641,
0.0382406263660542));
#18176=CARTESIAN_POINT('Ctrl Pts',(0.0924816165728724,0.0957056566670696,
0.0408272850023869));
#18177=CARTESIAN_POINT('Ctrl Pts',(0.0540676193498672,0.121610671661662,
0.0434139436387195));
#18178=CARTESIAN_POINT('Ctrl Pts',(0.0133639835211523,0.125930636937597,
0.0460006022750522));
#18179=CARTESIAN_POINT('Ctrl Pts',(-0.0273396523075625,0.130250602213533,
0.0485872609113848));
#18180=CARTESIAN_POINT('Ctrl Pts',(-0.0703329267419868,0.112985517770812,
0.0511739195477175));
#18181=CARTESIAN_POINT('Ctrl Pts',(-0.0967449447385466,0.0817152626609385,
0.0537605781840501));
#18182=CARTESIAN_POINT('Ctrl Pts',(-0.115741878896724,0.0592240248649833,
0.0556210412433473));
#18183=CARTESIAN_POINT('Ctrl Pts',(-0.126160906676814,0.0294875554882879,
0.0574815043026445));
#18184=CARTESIAN_POINT('Ctrl Pts',(-0.126396145829628,-9.95859796292312E-5,
0.0593419673619417));
#18185=CARTESIAN_POINT('Origin',(0.,0.,0.12));
#18186=CARTESIAN_POINT('',(-0.126529791093031,9.025049583615E-5,0.109341967361942));
#18187=CARTESIAN_POINT('',(-0.126349242904067,8.85860673823967E-5,0.0956580326380584));
#18188=CARTESIAN_POINT('',(-0.12645,1.54856587752183E-17,0.12));
#18189=CARTESIAN_POINT('Ctrl Pts',(-0.126349242904067,8.85860673823967E-5,
0.0956580326380584));
#18190=CARTESIAN_POINT('Ctrl Pts',(-0.126441591528965,0.0135570965972842,
0.0948119253946973));
#18191=CARTESIAN_POINT('Ctrl Pts',(-0.124448136217638,0.0269990101701626,
0.0939658181513361));
#18192=CARTESIAN_POINT('Ctrl Pts',(-0.120249444863787,0.0397126388809939,
0.093119710907975));
#18193=CARTESIAN_POINT('Ctrl Pts',(-0.107413505522824,0.0785798365820317,
0.0905330522716423));
#18194=CARTESIAN_POINT('Ctrl Pts',(-0.0739673525896496,0.110640458354997,
0.0879463936353097));
#18195=CARTESIAN_POINT('Ctrl Pts',(-0.0345920580258737,0.121821308595361,
0.085359734998977));
#18196=CARTESIAN_POINT('Ctrl Pts',(0.00478323653790218,0.133002158835724,
0.0827730763626444));
#18197=CARTESIAN_POINT('Ctrl Pts',(0.0500876727322792,0.123303237543486,
0.0801864177263117));
#18198=CARTESIAN_POINT('Ctrl Pts',(0.0814342209129887,0.0969820390626645,
0.077599759089979));
#18199=CARTESIAN_POINT('Ctrl Pts',(0.112780769093698,0.0706608405818426,
0.0750131004536464));
#18200=CARTESIAN_POINT('Ctrl Pts',(0.13016942926074,0.0277173649124373,
0.0724264418173139));
#18201=CARTESIAN_POINT('Ctrl Pts',(0.12596827751407,-0.0129984006283456,
0.0698397831809812));
#18202=CARTESIAN_POINT('Ctrl Pts',(0.121767125767399,-0.0537141661691284,
0.0672531245446486));
#18203=CARTESIAN_POINT('Ctrl Pts',(0.0959761621070158,-0.0922022215812886,
0.0646664659083159));
#18204=CARTESIAN_POINT('Ctrl Pts',(0.059914723710966,-0.111567668284471,
0.0620798072719833));
#18205=CARTESIAN_POINT('Ctrl Pts',(0.0238532853149157,-0.130933114987654,
0.0594931486356506));
#18206=CARTESIAN_POINT('Ctrl Pts',(-0.0224786278168013,-0.131175952981858,
0.056906489999318));
#18207=CARTESIAN_POINT('Ctrl Pts',(-0.0587401909579078,-0.112190380850839,
0.0543198313629853));
#18208=CARTESIAN_POINT('Ctrl Pts',(-0.0950017540990138,-0.0932048087198191,
0.0517331727266527));
#18209=CARTESIAN_POINT('Ctrl Pts',(-0.12119296724951,-0.0549908264635757,
0.0491465140903201));
#18210=CARTESIAN_POINT('Ctrl Pts',(-0.125823286774378,-0.0143210998620416,
0.0465598554539874));
#18211=CARTESIAN_POINT('Ctrl Pts',(-0.126361397696569,-0.0095946821776348,
0.0462592478486778));
#18212=CARTESIAN_POINT('Ctrl Pts',(-0.12660831057823,-0.00483509759607578,
0.0459586402433681));
#18213=CARTESIAN_POINT('Ctrl Pts',(-0.126575671592806,-7.20628672610732E-5,
0.0456580326380584));
#18214=CARTESIAN_POINT('Ctrl Pts',(-0.126396145829628,-9.95859796292312E-5,
0.0593419673619417));
#18215=CARTESIAN_POINT('Ctrl Pts',(-0.12648796685852,-0.0116483513064931,
0.0600681629389771));
#18216=CARTESIAN_POINT('Ctrl Pts',(-0.125028206814926,-0.0231743653405588,
0.0607943585160125));
#18217=CARTESIAN_POINT('Ctrl Pts',(-0.121921363946098,-0.034237873926493,
0.0615205540930479));
#18218=CARTESIAN_POINT('Ctrl Pts',(-0.110855003598394,-0.0736453296270277,
0.0641072127293806));
#18219=CARTESIAN_POINT('Ctrl Pts',(-0.0788915213442898,-0.107184815251071,
0.0666938713657133));
#18220=CARTESIAN_POINT('Ctrl Pts',(-0.0400617348236378,-0.120133683626334,
0.069280530002046));
#18221=CARTESIAN_POINT('Ctrl Pts',(-0.00123194830298627,-0.133082552001597,
0.0718671886383786));
#18222=CARTESIAN_POINT('Ctrl Pts',(0.0444641424842127,-0.125440803128081,
0.0744538472747112));
#18223=CARTESIAN_POINT('Ctrl Pts',(0.0769682295152699,-0.100563001286921,
0.0770405059110438));
#18224=CARTESIAN_POINT('Ctrl Pts',(0.109472316546327,-0.0756851994457607,
0.0796271645473764));
#18225=CARTESIAN_POINT('Ctrl Pts',(0.128784399821243,-0.0335713446369571,
0.0822138231837091));
#18226=CARTESIAN_POINT('Ctrl Pts',(0.126427276285523,0.00729262199647547,
0.0848004818200417));
#18227=CARTESIAN_POINT('Ctrl Pts',(0.124070152749803,0.0481565886299079,
0.0873871404563744));
#18228=CARTESIAN_POINT('Ctrl Pts',(0.100043822403448,0.0877706670879697,
0.0899737990927071));
#18229=CARTESIAN_POINT('Ctrl Pts',(0.0648947831756147,0.108746049780439,
0.0925604577290397));
#18230=CARTESIAN_POINT('Ctrl Pts',(0.0297457439477817,0.129721432472907,
0.0951471163653723));
#18231=CARTESIAN_POINT('Ctrl Pts',(-0.0165260041615291,0.132058119399784,
0.0977337750017049));
#18232=CARTESIAN_POINT('Ctrl Pts',(-0.0536093211433369,0.114730442741844,
0.100320433638038));
#18233=CARTESIAN_POINT('Ctrl Pts',(-0.0906926381251451,0.0974027660839045,
0.10290709227437));
#18234=CARTESIAN_POINT('Ctrl Pts',(-0.11858752397945,0.0604107258411485,
0.105493750910703));
#18235=CARTESIAN_POINT('Ctrl Pts',(-0.12504939731921,0.0199921027543164,
0.108080409547035));
#18236=CARTESIAN_POINT('Ctrl Pts',(-0.126099919499473,0.0134211506765118,
0.108500928818671));
#18237=CARTESIAN_POINT('Ctrl Pts',(-0.126583971845017,0.00675963476331471,
0.108921448090306));
#18238=CARTESIAN_POINT('Ctrl Pts',(-0.126529791093031,9.025049583615E-5,
0.109341967361942));
#18239=CARTESIAN_POINT('Origin',(0.,0.,0.12));
#18240=CARTESIAN_POINT('',(-0.126296536029262,-6.10717992316628E-5,0.159341967361942));
#18241=CARTESIAN_POINT('',(-0.126453631260982,-0.000102348163238207,0.145658032638058));
#18242=CARTESIAN_POINT('',(-0.12645,1.54856587752183E-17,0.12));
#18243=CARTESIAN_POINT('Ctrl Pts',(-0.126453631260982,-0.000102348163238207,
0.145658032638058));
#18244=CARTESIAN_POINT('Ctrl Pts',(-0.126183364177612,0.031552920325249,
0.143665210546026));
#18245=CARTESIAN_POINT('Ctrl Pts',(-0.114073771100105,0.0633928690595716,
0.141672388453994));
#18246=CARTESIAN_POINT('Ctrl Pts',(-0.0925489356314354,0.0864391430514358,
0.139679566361962));
#18247=CARTESIAN_POINT('Ctrl Pts',(-0.0646099631645552,0.116352924063146,
0.13709290772563));
#18248=CARTESIAN_POINT('Ctrl Pts',(-0.0208084524006029,0.131451366650306,
0.134506249089297));
#18249=CARTESIAN_POINT('Ctrl Pts',(0.0196287675426836,0.125106932552633,
0.131919590452964));
#18250=CARTESIAN_POINT('Ctrl Pts',(0.0600659874859703,0.11876249845496,
0.129332931816632));
#18251=CARTESIAN_POINT('Ctrl Pts',(0.097138916608591,0.0909751876724545,
0.126746273180299));
#18252=CARTESIAN_POINT('Ctrl Pts',(0.114574233156503,0.0539423598350403,
0.124159614543967));
#18253=CARTESIAN_POINT('Ctrl Pts',(0.132009549704415,0.0169095319976262,
0.121572955907634));
#18254=CARTESIAN_POINT('Ctrl Pts',(0.129807253677619,-0.0293688128946969,
0.118986297271301));
#18255=CARTESIAN_POINT('Ctrl Pts',(0.108934072954415,-0.0645786240759305,
0.116399638634969));
#18256=CARTESIAN_POINT('Ctrl Pts',(0.0880608922312115,-0.099788435257164,
0.113812979998636));
#18257=CARTESIAN_POINT('Ctrl Pts',(0.0485168268116012,-0.123929712727308,
0.111226321362303));
#18258=CARTESIAN_POINT('Ctrl Pts',(0.00765986125275547,-0.126405537442516,
0.108639662725971));
#18259=CARTESIAN_POINT('Ctrl Pts',(-0.0331971043060904,-0.128881362157723,
0.106053004089638));
#18260=CARTESIAN_POINT('Ctrl Pts',(-0.0753669700041717,-0.109691734117994,
0.103466345453305));
#18261=CARTESIAN_POINT('Ctrl Pts',(-0.100339039978837,-0.0772600332835736,
0.100879686816973));
#18262=CARTESIAN_POINT('Ctrl Pts',(-0.117142637704978,-0.0554368822612891,
0.0991391354240014));
#18263=CARTESIAN_POINT('Ctrl Pts',(-0.126159269908366,-0.0276178718881664,
0.0973985840310299));
#18264=CARTESIAN_POINT('Ctrl Pts',(-0.126349242904067,8.85860673823967E-5,
0.0956580326380584));
#18265=CARTESIAN_POINT('Ctrl Pts',(-0.126529791093031,9.025049583615E-5,
0.109341967361942));
#18266=CARTESIAN_POINT('Ctrl Pts',(-0.126250700293628,-0.0342644551610371,
0.111508106726639));
#18267=CARTESIAN_POINT('Ctrl Pts',(-0.111690189779818,-0.0688279388928191,
0.113674246091336));
#18268=CARTESIAN_POINT('Ctrl Pts',(-0.0867076257192948,-0.092297473337895,
0.115840385456033));
#18269=CARTESIAN_POINT('Ctrl Pts',(-0.0568751199544048,-0.120323220412367,
0.118427044092366));
#18270=CARTESIAN_POINT('Ctrl Pts',(-0.0121812475994092,-0.132529508630403,
0.121013702728699));
#18271=CARTESIAN_POINT('Ctrl Pts',(0.0277554439013372,-0.123558363290506,
0.123600361365031));
#18272=CARTESIAN_POINT('Ctrl Pts',(0.0676921354020838,-0.114587217950609,
0.126187020001364));
#18273=CARTESIAN_POINT('Ctrl Pts',(0.102871646048582,-0.0844386390527785,
0.128773678637697));
#18274=CARTESIAN_POINT('Ctrl Pts',(0.117851793294146,-0.0463464242807743,
0.131360337274029));
#18275=CARTESIAN_POINT('Ctrl Pts',(0.13283194053971,-0.00825420950877041,
0.133946995910362));
#18276=CARTESIAN_POINT('Ctrl Pts',(0.127612724384341,0.0377816411374068,
0.136533654546694));
#18277=CARTESIAN_POINT('Ctrl Pts',(0.104485135941302,0.0715534408109559,
0.139120313183027));
#18278=CARTESIAN_POINT('Ctrl Pts',(0.0813575474982633,0.105325240484505,
0.14170697181936));
#18279=CARTESIAN_POINT('Ctrl Pts',(0.0403215867675544,0.126832989185426,
0.144293630455692));
#18280=CARTESIAN_POINT('Ctrl Pts',(-0.000609841963000384,0.126635909896556,
0.146880289092025));
#18281=CARTESIAN_POINT('Ctrl Pts',(-0.0415412706935549,0.126438830607686,
0.149466947728358));
#18282=CARTESIAN_POINT('Ctrl Pts',(-0.0823681674239554,0.104536923329025,
0.15205360636469));
#18283=CARTESIAN_POINT('Ctrl Pts',(-0.10516942503222,0.0705438627883669,
0.154640265001023));
#18284=CARTESIAN_POINT('Ctrl Pts',(-0.118984510025511,0.0499477610899654,
0.156207499121329));
#18285=CARTESIAN_POINT('Ctrl Pts',(-0.126182304652747,0.0249129445447297,
0.157774733241635));
#18286=CARTESIAN_POINT('Ctrl Pts',(-0.126296536029262,-6.10717992316628E-5,
0.159341967361942));
#18287=CARTESIAN_POINT('Origin',(0.,0.,0.12));
#18288=CARTESIAN_POINT('',(-0.126625441102054,2.7778768752873E-5,0.209341967361942));
#18289=CARTESIAN_POINT('',(-0.126471935391749,0.000101176582396995,0.195658032638058));
#18290=CARTESIAN_POINT('',(-0.12645,1.54856587752183E-17,0.12));
#18291=CARTESIAN_POINT('',(0.0958116152722397,0.0825211298936481,0.24));
#18292=CARTESIAN_POINT('Ctrl Pts',(-0.126625441102054,2.7778768752873E-5,
0.209341967361942));
#18293=CARTESIAN_POINT('Ctrl Pts',(-0.126482885932031,-0.0388928622545336,
0.21180133566563));
#18294=CARTESIAN_POINT('Ctrl Pts',(-0.107125339127294,-0.077921419747323,
0.214260703969318));
#18295=CARTESIAN_POINT('Ctrl Pts',(-0.0759952538809665,-0.101287130411732,
0.216720072273006));
#18296=CARTESIAN_POINT('Ctrl Pts',(-0.0432539585932993,-0.12586218783339,
0.219306730909339));
#18297=CARTESIAN_POINT('Ctrl Pts',(0.0025100419330305,-0.133111106253138,
0.221893389545672));
#18298=CARTESIAN_POINT('Ctrl Pts',(0.0412155518054008,-0.119764891216682,
0.224480048182004));
#18299=CARTESIAN_POINT('Ctrl Pts',(0.0799210616777711,-0.106418676180227,
0.227066706818337));
#18300=CARTESIAN_POINT('Ctrl Pts',(0.111568080896182,-0.072477327687567,
0.229653365454669));
#18301=CARTESIAN_POINT('Ctrl Pts',(0.122246574267713,-0.0330282462555153,
0.232240024091002));
#18302=CARTESIAN_POINT('Ctrl Pts',(0.132925067639245,0.00642083517653631,
0.234826682727335));
#18303=CARTESIAN_POINT('Ctrl Pts',(0.122635035163896,0.0513776495479799,
0.237413341363667));
#18304=CARTESIAN_POINT('Ctrl Pts',(0.0958116152722397,0.0825211298936481,
0.24));
#18305=CARTESIAN_POINT('',(-0.0959791030802601,0.0826138105732953,0.24));
#18306=CARTESIAN_POINT('Origin',(0.,0.,0.24));
#18307=CARTESIAN_POINT('Ctrl Pts',(-0.0959791030802601,0.0826138105732953,
0.24));
#18308=CARTESIAN_POINT('Ctrl Pts',(-0.0710417758635208,0.111296717646776,
0.237599759089979));
#18309=CARTESIAN_POINT('Ctrl Pts',(-0.0322351762885183,0.128218895525122,
0.235199518179958));
#18310=CARTESIAN_POINT('Ctrl Pts',(0.00571352152256588,0.126497857083363,
0.232799277269937));
#18311=CARTESIAN_POINT('Ctrl Pts',(0.0466095526337785,0.124643152028446,
0.230212618633605));
#18312=CARTESIAN_POINT('Ctrl Pts',(0.0865092470399708,0.101136876245298,
0.227625959997272));
#18313=CARTESIAN_POINT('Ctrl Pts',(0.107920636628548,0.0662586835305903,
0.225039301360939));
#18314=CARTESIAN_POINT('Ctrl Pts',(0.129332026217125,0.0313804908158828,
0.222452642724607));
#18315=CARTESIAN_POINT('Ctrl Pts',(0.132255110988087,-0.014869618830384,
0.219865984088274));
#18316=CARTESIAN_POINT('Ctrl Pts',(0.115395215428634,-0.0521699181865619,
0.217279325451942));
#18317=CARTESIAN_POINT('Ctrl Pts',(0.0985353198691812,-0.0894702175427398,
0.214692666815609));
#18318=CARTESIAN_POINT('Ctrl Pts',(0.0618924439793129,-0.117820706608829,
0.212106008179276));
#18319=CARTESIAN_POINT('Ctrl Pts',(0.0215571925812854,-0.12478734248304,
0.209519349542944));
#18320=CARTESIAN_POINT('Ctrl Pts',(-0.0187780588167422,-0.13175397835725,
0.206932690906611));
#18321=CARTESIAN_POINT('Ctrl Pts',(-0.0628056857229291,-0.117336761039583,
0.204346032270278));
#18322=CARTESIAN_POINT('Ctrl Pts',(-0.0912027768750998,-0.0878586653637446,
0.201759373633946));
#18323=CARTESIAN_POINT('Ctrl Pts',(-0.113530209130371,-0.0646812849521466,
0.199725593301983));
#18324=CARTESIAN_POINT('Ctrl Pts',(-0.126194825294183,-0.0321932513395888,
0.197691812970021));
#18325=CARTESIAN_POINT('Ctrl Pts',(-0.126471935391749,0.000101176582396995,
0.195658032638058));
#18326=CARTESIAN_POINT('Origin',(0.,0.,0.350421172358873));
#18327=CARTESIAN_POINT('',(-0.154453350152392,-8.79343647196378E-5,0.0295788276411275));
#18328=CARTESIAN_POINT('',(-0.15422847552802,0.000108763211052777,0.025421172358873));
#18329=CARTESIAN_POINT('',(-0.1543,-1.01731279388251E-15,0.350421172358873));
#18330=CARTESIAN_POINT('',(0.15408394018464,-0.00816268198427004,0.));
#18331=CARTESIAN_POINT('Ctrl Pts',(-0.15422847552802,0.000108763211052763,
0.025421172358873));
#18332=CARTESIAN_POINT('Ctrl Pts',(-0.154338737393477,0.0139570514561378,
0.0247074241482466));
#18333=CARTESIAN_POINT('Ctrl Pts',(-0.146387882101843,0.0778735560251454,
0.0214070173012875));
#18334=CARTESIAN_POINT('Ctrl Pts',(-0.0581466660421577,0.171532975008042,
0.0155199518179959));
#18335=CARTESIAN_POINT('Ctrl Pts',(0.109502662757235,0.144085240745689,
0.00775997590899784));
#18336=CARTESIAN_POINT('Ctrl Pts',(0.156737212705124,0.0419221657566679,
0.00258665863633264));
#18337=CARTESIAN_POINT('Ctrl Pts',(0.15408394018464,-0.00816268198427004,
0.));
#18338=CARTESIAN_POINT('',(0.129620323775263,-0.0841289546921688,3.62607491890453E-17));
#18339=CARTESIAN_POINT('Origin',(0.,0.,0.));
#18340=CARTESIAN_POINT('Ctrl Pts',(-0.154453350152392,-8.7934364719636E-5,
0.0295788276411275));
#18341=CARTESIAN_POINT('Ctrl Pts',(-0.154150470777978,0.0441115087317509,
0.0272927766101045));
#18342=CARTESIAN_POINT('Ctrl Pts',(-0.111454882743928,0.138841433785012,
0.0224200669427489));
#18343=CARTESIAN_POINT('Ctrl Pts',(0.0476444145610997,0.174632482457551,
0.0149606986390605));
#18344=CARTESIAN_POINT('Ctrl Pts',(0.168251138196633,0.0613688951001999,
0.0073871404563744));
#18345=CARTESIAN_POINT('Ctrl Pts',(0.154676764047789,-0.0451013867871701,
0.00240024091002087));
#18346=CARTESIAN_POINT('Ctrl Pts',(0.129620323775263,-0.0841289546921688,
1.57209315010398E-17));
#18347=CARTESIAN_POINT('Origin',(0.,0.,0.350421172358873));
#18348=CARTESIAN_POINT('',(-0.154177051641736,0.000108096719625833,0.0795788276411275));
#18349=CARTESIAN_POINT('',(-0.154234284709463,-0.000121519309271207,0.075421172358873));
#18350=CARTESIAN_POINT('',(-0.1543,-1.01731279388251E-15,0.350421172358873));
#18351=CARTESIAN_POINT('Ctrl Pts',(-0.154234284709463,-0.000121519309271208,
0.0754211723588731));
#18352=CARTESIAN_POINT('Ctrl Pts',(-0.153947235272697,0.0359820467524117,
0.0735607092995758));
#18353=CARTESIAN_POINT('Ctrl Pts',(-0.123557126730793,0.122717061869437,
0.0691135876039459));
#18354=CARTESIAN_POINT('Ctrl Pts',(0.0191012565771036,0.180005302104073,
0.0620798072719832));
#18355=CARTESIAN_POINT('Ctrl Pts',(0.159724738700703,0.0851738948996701,
0.0543198313629854));
#18356=CARTESIAN_POINT('Ctrl Pts',(0.160113920417758,-0.0844204212478698,
0.0465598554539874));
#18357=CARTESIAN_POINT('Ctrl Pts',(0.0199582426985643,-0.179924098035372,
0.0387998795449896));
#18358=CARTESIAN_POINT('Ctrl Pts',(-0.123251388539896,-0.123176028715441,
0.0317536518466181));
#18359=CARTESIAN_POINT('Ctrl Pts',(-0.153939142967466,-0.0362298265692857,
0.0272940827845792));
#18360=CARTESIAN_POINT('Ctrl Pts',(-0.15422847552802,0.000108763211052763,
0.025421172358873));
#18361=CARTESIAN_POINT('Ctrl Pts',(-0.154177051641736,0.000108096719625859,
0.0795788276411275));
#18362=CARTESIAN_POINT('Ctrl Pts',(-0.154289739603949,0.0165429814548096,
0.0787327203977663));
#18363=CARTESIAN_POINT('Ctrl Pts',(-0.144420757340354,0.0830897487115299,
0.0752999545180725));
#18364=CARTESIAN_POINT('Ctrl Pts',(-0.0494457976037486,0.174130301808973,
0.0692805300020459));
#18365=CARTESIAN_POINT('Ctrl Pts',(0.11640175885633,0.13862511662766,0.061520554093048));
#18366=CARTESIAN_POINT('Ctrl Pts',(0.18005704388064,-0.0185795878987759,
0.0537605781840501));
#18367=CARTESIAN_POINT('Ctrl Pts',(0.0856431484406112,-0.159474177462153,
0.0460006022750521));
#18368=CARTESIAN_POINT('Ctrl Pts',(-0.0839657292871194,-0.160363143120653,
0.0382406263660544));
#18369=CARTESIAN_POINT('Ctrl Pts',(-0.151599316432495,-0.0616831513139142,
0.0327667014880793));
#18370=CARTESIAN_POINT('Ctrl Pts',(-0.154493177716258,-0.00590000442131094,
0.0298794352464371));
#18371=CARTESIAN_POINT('Ctrl Pts',(-0.154453350152392,-8.7934364719636E-5,
0.0295788276411275));
#18372=CARTESIAN_POINT('Origin',(0.,0.,0.350421172358873));
#18373=CARTESIAN_POINT('',(-0.154304431028624,-0.000124889850439479,0.129578827641127));
#18374=CARTESIAN_POINT('',(-0.154397364694779,0.000110127730384366,0.125421172358873));
#18375=CARTESIAN_POINT('',(-0.1543,-1.01731279388251E-15,0.350421172358873));
#18376=CARTESIAN_POINT('Ctrl Pts',(-0.154397364694779,0.000110127730384357,
0.125421172358873));
#18377=CARTESIAN_POINT('Ctrl Pts',(-0.154463478494948,0.00824841157753406,
0.125000653087238));
#18378=CARTESIAN_POINT('Ctrl Pts',(-0.150239588102603,0.0663774823757793,
0.121993475179269));
#18379=CARTESIAN_POINT('Ctrl Pts',(-0.0766286530280003,0.163994611436961,
0.116399638634969));
#18380=CARTESIAN_POINT('Ctrl Pts',(0.0927599764682439,0.155440618724813,
0.108639662725971));
#18381=CARTESIAN_POINT('Ctrl Pts',(0.180714016146597,0.0104239566588842,
0.100879686816973));
#18382=CARTESIAN_POINT('Ctrl Pts',(0.11001758793024,-0.143743725357685,
0.093119710907975));
#18383=CARTESIAN_POINT('Ctrl Pts',(-0.0572637123892103,-0.171718146500831,
0.0853597349989769));
#18384=CARTESIAN_POINT('Ctrl Pts',(-0.146220320052713,-0.0783754111826042,
0.0794602221492764));
#18385=CARTESIAN_POINT('Ctrl Pts',(-0.154346328875204,-0.0142138442593302,
0.0761473679359084));
#18386=CARTESIAN_POINT('Ctrl Pts',(-0.154234284709463,-0.000121519309271208,
0.0754211723588731));
#18387=CARTESIAN_POINT('Ctrl Pts',(-0.154304431028624,-0.000124889850439474,
0.129578827641127));
#18388=CARTESIAN_POINT('Ctrl Pts',(-0.153974638929265,0.0385022981904757,
0.127586005549095));
#18389=CARTESIAN_POINT('Ctrl Pts',(-0.120018027207353,0.127784966030512,
0.123006524820731));
#18390=CARTESIAN_POINT('Ctrl Pts',(0.0280571680938306,0.178826694862324,
0.115840385456033));
#18391=CARTESIAN_POINT('Ctrl Pts',(0.163771354656592,0.0771047007047774,
0.108080409547035));
#18392=CARTESIAN_POINT('Ctrl Pts',(0.155709331479018,-0.0923080778690166,
0.100320433638038));
#18393=CARTESIAN_POINT('Ctrl Pts',(0.0109489686262093,-0.180682908560435,
0.0925604577290397));
#18394=CARTESIAN_POINT('Ctrl Pts',(-0.126591758993125,-0.118094248159534,
0.0856465890634029));
#18395=CARTESIAN_POINT('Ctrl Pts',(-0.153945238013925,-0.0337005743957639,
0.0813193790340989));
#18396=CARTESIAN_POINT('Ctrl Pts',(-0.154177051641736,0.000108096719625859,
0.0795788276411275));
#18397=CARTESIAN_POINT('Origin',(0.,0.,0.350421172358873));
#18398=CARTESIAN_POINT('',(-0.154326766555531,0.000123460234585843,0.179578827641127));
#18399=CARTESIAN_POINT('',(-0.154112736333057,-7.45225671948511E-5,0.175421172358873));
#18400=CARTESIAN_POINT('',(-0.1543,-1.01731279388251E-15,0.350421172358873));
#18401=CARTESIAN_POINT('Ctrl Pts',(-0.154112736333057,-7.45225671948471E-5,
0.175421172358873));
#18402=CARTESIAN_POINT('Ctrl Pts',(-0.153973346049181,0.0303998999070902,
0.173853938238567));
#18403=CARTESIAN_POINT('Ctrl Pts',(-0.130694151755309,0.111367805862998,
0.169700045481928));
#18404=CARTESIAN_POINT('Ctrl Pts',(-0.000871711368246156,0.181012066871201,
0.162959494088956));
#18405=CARTESIAN_POINT('Ctrl Pts',(0.149350085565286,0.102277888352765,
0.155199518179958));
#18406=CARTESIAN_POINT('Ctrl Pts',(0.168456255263351,-0.0662471829332422,
0.14743954227096));
#18407=CARTESIAN_POINT('Ctrl Pts',(0.0396733728729688,-0.17661315503135,
0.139679566361963));
#18408=CARTESIAN_POINT('Ctrl Pts',(-0.115072782317819,-0.134350623919955,
0.1323401097246));
#18409=CARTESIAN_POINT('Ctrl Pts',(-0.154056805498669,-0.041811035439686,
0.12758731172357));
#18410=CARTESIAN_POINT('Ctrl Pts',(-0.154397364694779,0.000110127730384357,
0.125421172358873));
#18411=CARTESIAN_POINT('Ctrl Pts',(-0.154326766555531,0.000123460234585825,
0.179578827641127));
#18412=CARTESIAN_POINT('Ctrl Pts',(-0.154418689716183,0.0108361910665024,
0.179025949336757));
#18413=CARTESIAN_POINT('Ctrl Pts',(-0.148597337680631,0.071569631208062,
0.175886412396054));
#18414=CARTESIAN_POINT('Ctrl Pts',(-0.0683530255288039,0.167611467503216,
0.170160216819019));
#18415=CARTESIAN_POINT('Ctrl Pts',(0.100397202365132,0.150621028353064,
0.162400240910021));
#18416=CARTESIAN_POINT('Ctrl Pts',(0.18100910679194,0.00139719974911195,
0.154640265001023));
#18417=CARTESIAN_POINT('Ctrl Pts',(0.102711092909207,-0.149052183789333,
0.146880289092025));
#18418=CARTESIAN_POINT('Ctrl Pts',(-0.0657574679958034,-0.168648048308422,
0.139120313183027));
#18419=CARTESIAN_POINT('Ctrl Pts',(-0.148058381688037,-0.0731761882111772,
0.133353159366061));
#18420=CARTESIAN_POINT('Ctrl Pts',(-0.154402705029802,-0.0116353181791797,
0.130172664185428));
#18421=CARTESIAN_POINT('Ctrl Pts',(-0.154304431028624,-0.000124889850439474,
0.129578827641127));
#18422=CARTESIAN_POINT('Origin',(0.,0.,0.350421172358873));
#18423=CARTESIAN_POINT('',(-0.154128406284035,-0.000157308197905263,0.229578827641128));
#18424=CARTESIAN_POINT('',(-0.154514081154978,3.38969080117728E-5,0.225421172358873));
#18425=CARTESIAN_POINT('',(-0.1543,-1.01731279388251E-15,0.350421172358873));
#18426=CARTESIAN_POINT('',(-0.0398513841857245,-0.149064942821851,0.24));
#18427=CARTESIAN_POINT('Ctrl Pts',(-0.0398513841857245,-0.149064942821851,
0.24));
#18428=CARTESIAN_POINT('Ctrl Pts',(-0.0883048112969314,-0.136111285829332,
0.237413341363667));
#18429=CARTESIAN_POINT('Ctrl Pts',(-0.143745772087175,-0.0847488633265083,
0.233939617244043));
#18430=CARTESIAN_POINT('Ctrl Pts',(-0.154234229255939,-0.017399338864059,
0.230465893124419));
#18431=CARTESIAN_POINT('Ctrl Pts',(-0.154128406284035,-0.00015730819790527,
0.229578827641128));
#18432=CARTESIAN_POINT('',(0.0399565498027962,-0.149273502906638,0.24));
#18433=CARTESIAN_POINT('Origin',(0.,0.,0.24));
#18434=CARTESIAN_POINT('Ctrl Pts',(0.0399565498027963,-0.149273502906638,
0.24));
#18435=CARTESIAN_POINT('Ctrl Pts',(-0.00490373130458673,-0.161043406468747,
0.237599759089979));
#18436=CARTESIAN_POINT('Ctrl Pts',(-0.107666111297752,-0.141562671532916,
0.23274014987627));
#18437=CARTESIAN_POINT('Ctrl Pts',(-0.154340128899266,-0.0474588267763927,
0.227880540662561));
#18438=CARTESIAN_POINT('Ctrl Pts',(-0.154514081154978,3.3896908011755E-5,
0.225421172358873));
#18439=CARTESIAN_POINT('Origin',(0.,0.,0.350421172358873));
#18440=CARTESIAN_POINT('Ctrl Pts',(-0.154514081154978,3.3896908011755E-5,
0.225421172358873));
#18441=CARTESIAN_POINT('Ctrl Pts',(-0.154523084458981,0.00249199339844659,
0.225293882026228));
#18442=CARTESIAN_POINT('Ctrl Pts',(-0.153375868586475,0.0548933889046004,
0.222579933057251));
#18443=CARTESIAN_POINT('Ctrl Pts',(-0.0942515706791253,0.154556313135293,
0.217279325451942));
#18444=CARTESIAN_POINT('Ctrl Pts',(0.0750450248431312,0.164716481511431,
0.209519349542944));
#18445=CARTESIAN_POINT('Ctrl Pts',(0.178461260043253,0.0303012077178856,
0.201759373633945));
#18446=CARTESIAN_POINT('Ctrl Pts',(0.125203781387627,-0.130731709675357,
0.193999397724948));
#18447=CARTESIAN_POINT('Ctrl Pts',(-0.0379704533096903,-0.17698585337688,
0.18623942181595));
#18448=CARTESIAN_POINT('Ctrl Pts',(-0.141587477595567,-0.0899051669249145,
0.180046680027258));
#18449=CARTESIAN_POINT('Ctrl Pts',(-0.154203404262525,-0.019896942829432,
0.176440596874899));
#18450=CARTESIAN_POINT('Ctrl Pts',(-0.154112736333057,-7.45225671948471E-5,
0.175421172358873));
#18451=CARTESIAN_POINT('Ctrl Pts',(-0.154128406284035,-0.00015730819790527,
0.229578827641128));
#18452=CARTESIAN_POINT('Ctrl Pts',(-0.153925652370292,0.0328779499839183,
0.227879234488086));
#18453=CARTESIAN_POINT('Ctrl Pts',(-0.127638532780061,0.116591914860373,
0.223592982698713));
#18454=CARTESIAN_POINT('Ctrl Pts',(0.00818767200092134,0.180778621679153,
0.216720072273006));
#18455=CARTESIAN_POINT('Ctrl Pts',(0.154249898498561,0.0947283641859207,
0.208960096364008));
#18456=CARTESIAN_POINT('Ctrl Pts',(0.164950538597243,-0.0745810526211722,
0.201200120455011));
#18457=CARTESIAN_POINT('Ctrl Pts',(0.0308106631569891,-0.178364693496558,
0.193440144546012));
#18458=CARTESIAN_POINT('Ctrl Pts',(-0.118879635670858,-0.129347344159377,
0.186233046941385));
#18459=CARTESIAN_POINT('Ctrl Pts',(-0.153988624301243,-0.0392836590090855,
0.18161260797309));
#18460=CARTESIAN_POINT('Ctrl Pts',(-0.154326766555531,0.000123460234585825,
0.179578827641127));
#18461=CARTESIAN_POINT('Ctrl Pts',(0.0958116152722397,0.0825211298936481,
0.24));
#18462=CARTESIAN_POINT('Ctrl Pts',(0.122635035163896,0.0513776495479799,
0.237413341363667));
#18463=CARTESIAN_POINT('Ctrl Pts',(0.143215100114593,-0.0385359791949074,
0.232240024091002));
#18464=CARTESIAN_POINT('Ctrl Pts',(0.0482740424593604,-0.140360024672886,
0.224480048182004));
#18465=CARTESIAN_POINT('Ctrl Pts',(-0.0890179591196291,-0.118613269413641,
0.216720072273006));
#18466=CARTESIAN_POINT('Ctrl Pts',(-0.148173729266643,0.00709031985706173,
0.208960096364008));
#18467=CARTESIAN_POINT('Ctrl Pts',(-0.0772398646297824,0.126660050524678,
0.20120012045501));
#18468=CARTESIAN_POINT('Ctrl Pts',(0.0614999571705377,0.134986384232796,
0.193440144546013));
#18469=CARTESIAN_POINT('Ctrl Pts',(0.146250332679645,0.0248320655601208,
0.185680168637014));
#18470=CARTESIAN_POINT('Ctrl Pts',(0.102605431992647,-0.107135610424167,
0.177920192728017));
#18471=CARTESIAN_POINT('Ctrl Pts',(-0.0311170694815965,-0.145041225920327,
0.170160216819019));
#18472=CARTESIAN_POINT('Ctrl Pts',(-0.137521919612742,-0.0556176253575994,
0.162400240910021));
#18473=CARTESIAN_POINT('Ctrl Pts',(-0.123195064154356,0.0826350160503635,
0.154640265001023));
#18474=CARTESIAN_POINT('Ctrl Pts',(-0.000714373963154436,0.148340737886347,
0.146880289092025));
#18475=CARTESIAN_POINT('Ctrl Pts',(0.122393508228972,0.0838174917835845,
0.139120313183027));
#18476=CARTESIAN_POINT('Ctrl Pts',(0.138051156695079,-0.0542900601549481,
0.131360337274029));
#18477=CARTESIAN_POINT('Ctrl Pts',(0.032512624755586,-0.14473579684844,
0.123600361365031));
#18478=CARTESIAN_POINT('Ctrl Pts',(-0.101568992309399,-0.108116932194331,
0.115840385456033));
#18479=CARTESIAN_POINT('Ctrl Pts',(-0.146482409833755,0.0234186855983926,
0.108080409547036));
#18480=CARTESIAN_POINT('Ctrl Pts',(-0.0627977522708403,0.13439480632666,
0.100320433638038));
#18481=CARTESIAN_POINT('Ctrl Pts',(0.076017492057093,0.127384745546031,
0.0925604577290397));
#18482=CARTESIAN_POINT('Ctrl Pts',(0.148096483096158,0.00854251017184644,
0.0848004818200417));
#18483=CARTESIAN_POINT('Ctrl Pts',(0.0901602332714121,-0.117799054254564,
0.0770405059110438));
#18484=CARTESIAN_POINT('Ctrl Pts',(-0.0469280390901857,-0.140724300875114,
0.069280530002046));
#18485=CARTESIAN_POINT('Ctrl Pts',(-0.142818485852497,-0.0401058440029853,
0.0615205540930479));
#18486=CARTESIAN_POINT('Ctrl Pts',(-0.113326201176411,0.0957204333280909,
0.0537605781840501));
#18487=CARTESIAN_POINT('Ctrl Pts',(0.0156536221268617,0.147515686656254,
0.0460006022750521));
#18488=CARTESIAN_POINT('Ctrl Pts',(0.130895613795878,0.0698006416724775,
0.0382406263660543));
#18489=CARTESIAN_POINT('Ctrl Pts',(0.13121455111358,-0.0691831643991777,
0.0304806504570563));
#18490=CARTESIAN_POINT('Ctrl Pts',(0.0163559286405278,-0.147449139316739,
0.0227206745480584));
#18491=CARTESIAN_POINT('Ctrl Pts',(-0.112893560070904,-0.0962328986104914,
0.0149606986390606));
#18492=CARTESIAN_POINT('Ctrl Pts',(-0.142972035491037,0.0393992613429074,
0.00720072273006258));
#18493=CARTESIAN_POINT('Ctrl Pts',(-0.0476516261894416,0.140572551456688,
-0.000559253178935252));
#18494=CARTESIAN_POINT('Ctrl Pts',(0.0897382482543901,0.118078928660352,
-0.00831922908793326));
#18495=CARTESIAN_POINT('Ctrl Pts',(0.128447313976429,0.0343555272840613,
-0.0134925463605985));
#18496=CARTESIAN_POINT('Ctrl Pts',(0.126272937371016,-0.00668937872268922,
-0.0160792049969311));
#18497=CARTESIAN_POINT('Ctrl Pts',(0.102845629995666,0.0885794229410663,
0.245359734998977));
#18498=CARTESIAN_POINT('Ctrl Pts',(0.13163829265517,0.0551495423644061,
0.242773076362644));
#18499=CARTESIAN_POINT('Ctrl Pts',(0.153729244145676,-0.0413651001137901,
0.237599759089979));
#18500=CARTESIAN_POINT('Ctrl Pts',(0.0518180837997932,-0.150664563191773,
0.229839783180981));
#18501=CARTESIAN_POINT('Ctrl Pts',(-0.0955532172229155,-0.127321268762976,
0.222079807271983));
#18502=CARTESIAN_POINT('Ctrl Pts',(-0.159051911315084,0.00761085605850937,
0.214319831362985));
#18503=CARTESIAN_POINT('Ctrl Pts',(-0.0829104333128967,0.135958804728216,
0.206559855453988));
#18504=CARTESIAN_POINT('Ctrl Pts',(0.0660149797280689,0.144896416659008,
0.19879987954499));
#18505=CARTESIAN_POINT('Ctrl Pts',(0.156987308467515,0.0266551129460425,
0.191039903635992));
#18506=CARTESIAN_POINT('Ctrl Pts',(0.110138215124307,-0.11500097684123,
0.183279927726994));
#18507=CARTESIAN_POINT('Ctrl Pts',(-0.0334015307576278,-0.155689435072511,
0.175519951817996));
#18508=CARTESIAN_POINT('Ctrl Pts',(-0.147618098500879,-0.0597007962188336,
0.167759975908998));
#18509=CARTESIAN_POINT('Ctrl Pts',(-0.13223943620312,0.0887016700559064,
0.16));
#18510=CARTESIAN_POINT('Ctrl Pts',(-0.000766819764851659,0.159231180881298,
0.152240024091002));
#18511=CARTESIAN_POINT('Ctrl Pts',(0.131379034007743,0.0899709573066447,
0.144480048182004));
#18512=CARTESIAN_POINT('Ctrl Pts',(0.14818618955117,-0.0582757677477129,
0.136720072273006));
#18513=CARTESIAN_POINT('Ctrl Pts',(0.0348995407947136,-0.15536158290941,
0.128960096364009));
#18514=CARTESIAN_POINT('Ctrl Pts',(-0.109025685167754,-0.116054342400242,
0.12120012045501));
#18515=CARTESIAN_POINT('Ctrl Pts',(-0.157236423577976,0.0251379696208395,
0.113440144546013));
#18516=CARTESIAN_POINT('Ctrl Pts',(-0.0674080525232269,0.144261408030094,
0.105680168637014));
#18517=CARTESIAN_POINT('Ctrl Pts',(0.0815983201941432,0.136736703272292,
0.0979201927280168));
#18518=CARTESIAN_POINT('Ctrl Pts',(0.158968994112971,0.00916965900085902,
0.0901602168190187));
#18519=CARTESIAN_POINT('Ctrl Pts',(0.0967793514910216,-0.126447277955604,
0.0824002409100209));
#18520=CARTESIAN_POINT('Ctrl Pts',(-0.0503732635231939,-0.151055582750353,
0.0746402650010229));
#18521=CARTESIAN_POINT('Ctrl Pts',(-0.15330351242688,-0.0430502166284845,
0.066880289092025));
#18522=CARTESIAN_POINT('Ctrl Pts',(-0.121646050135849,0.102747753924341,
0.0591203131830272));
#18523=CARTESIAN_POINT('Ctrl Pts',(0.0168028336102756,0.158345558472194,
0.0513603372740292));
#18524=CARTESIAN_POINT('Ctrl Pts',(0.140505322097486,0.074925059414875,
0.0436003613650313));
#18525=CARTESIAN_POINT('Ctrl Pts',(0.140847674214973,-0.0742622500154084,
0.0358403854560334));
#18526=CARTESIAN_POINT('Ctrl Pts',(0.0175566999932067,-0.158274125556283,
0.0280804095470355));
#18527=CARTESIAN_POINT('Ctrl Pts',(-0.121181646661057,-0.103297841872129,
0.0203204336380376));
#18528=CARTESIAN_POINT('Ctrl Pts',(-0.153468334920127,0.0422917601656304,
0.0125604577290396));
#18529=CARTESIAN_POINT('Ctrl Pts',(-0.0511499728070136,0.150892692640473,
0.00480048182004178));
#18530=CARTESIAN_POINT('Ctrl Pts',(0.0963263864220051,0.126747699355464,
-0.00295949408895622));
#18531=CARTESIAN_POINT('Ctrl Pts',(0.137877280219327,0.0368777401082635,
-0.00813281136162143));
#18532=CARTESIAN_POINT('Ctrl Pts',(0.135543271642224,-0.00718047980988283,
-0.0107194699979541));
#18533=CARTESIAN_POINT('Ctrl Pts',(0.109879644719093,0.0946377159884845,
0.250719469997954));
#18534=CARTESIAN_POINT('Ctrl Pts',(0.140641550146443,0.0589214351808321,
0.248132811361621));
#18535=CARTESIAN_POINT('Ctrl Pts',(0.164243388176759,-0.0441942210326729,
0.242959494088956));
#18536=CARTESIAN_POINT('Ctrl Pts',(0.055362125140226,-0.160969101710661,
0.235199518179958));
#18537=CARTESIAN_POINT('Ctrl Pts',(-0.102088475326202,-0.13602926811231,
0.227439542270961));
#18538=CARTESIAN_POINT('Ctrl Pts',(-0.169930093363525,0.00813139225995705,
0.219679566361962));
#18539=CARTESIAN_POINT('Ctrl Pts',(-0.0885810019960112,0.145257558931755,
0.211919590452965));
#18540=CARTESIAN_POINT('Ctrl Pts',(0.0705300022856002,0.154806449085219,
0.204159614543967));
#18541=CARTESIAN_POINT('Ctrl Pts',(0.167724284255384,0.0284781603319641,
0.196399638634969));
#18542=CARTESIAN_POINT('Ctrl Pts',(0.117670998255967,-0.122866343258294,
0.188639662725971));
#18543=CARTESIAN_POINT('Ctrl Pts',(-0.0356859920336591,-0.166337644224695,
0.180879686816973));
#18544=CARTESIAN_POINT('Ctrl Pts',(-0.157714277389017,-0.0637839670800676,
0.173119710907975));
#18545=CARTESIAN_POINT('Ctrl Pts',(-0.141283808251885,0.0947683240614489,
0.165359734998977));
#18546=CARTESIAN_POINT('Ctrl Pts',(-0.000819265566548849,0.17012162387625,
0.157599759089979));
#18547=CARTESIAN_POINT('Ctrl Pts',(0.140364559786514,0.0961244228297045,
0.149839783180981));
#18548=CARTESIAN_POINT('Ctrl Pts',(0.158321222407261,-0.0622614753404775,
0.142079807271983));
#18549=CARTESIAN_POINT('Ctrl Pts',(0.0372864568338413,-0.16598736897038,
0.134319831362986));
#18550=CARTESIAN_POINT('Ctrl Pts',(-0.116482378026109,-0.123991752606152,
0.126559855453987));
#18551=CARTESIAN_POINT('Ctrl Pts',(-0.167990437322196,0.0268572536432864,
0.11879987954499));
#18552=CARTESIAN_POINT('Ctrl Pts',(-0.0720183527756138,0.154128009733527,
0.111039903635992));
#18553=CARTESIAN_POINT('Ctrl Pts',(0.0871791483311938,0.146088660998552,
0.103279927726994));
#18554=CARTESIAN_POINT('Ctrl Pts',(0.169841505129784,0.00979680782987164,
0.0955199518179957));
#18555=CARTESIAN_POINT('Ctrl Pts',(0.103398469710631,-0.135095501656644,
0.0877599759089979));
#18556=CARTESIAN_POINT('Ctrl Pts',(-0.0538184879562023,-0.161386864625592,
0.08));
#18557=CARTESIAN_POINT('Ctrl Pts',(-0.163788539001263,-0.0459945892539838,
0.0722400240910021));
#18558=CARTESIAN_POINT('Ctrl Pts',(-0.129965899095288,0.10977507452059,
0.0644800481820042));
#18559=CARTESIAN_POINT('Ctrl Pts',(0.0179520450936897,0.169175430288133,
0.0567200722730062));
#18560=CARTESIAN_POINT('Ctrl Pts',(0.150115030399095,0.0800494771572726,
0.0489600963640084));
#18561=CARTESIAN_POINT('Ctrl Pts',(0.150480797316365,-0.0793413356316391,
0.0412001204550104));
#18562=CARTESIAN_POINT('Ctrl Pts',(0.0187574713458855,-0.169099111795828,
0.0334401445460125));
#18563=CARTESIAN_POINT('Ctrl Pts',(-0.129469733251211,-0.110362785133767,
0.0256801686370146));
#18564=CARTESIAN_POINT('Ctrl Pts',(-0.163964634349217,0.0451842589883535,
0.0179201927280167));
#18565=CARTESIAN_POINT('Ctrl Pts',(-0.0546483194245858,0.161212833824257,
0.0101602168190188));
#18566=CARTESIAN_POINT('Ctrl Pts',(0.10291452458962,0.135416470050577,0.00240024091002082));
#18567=CARTESIAN_POINT('Ctrl Pts',(0.147307246462226,0.0393999529324658,
-0.00277307636264439));
#18568=CARTESIAN_POINT('Ctrl Pts',(0.144813605913432,-0.00767158089707644,
-0.00535973499897704));
#18569=CARTESIAN_POINT('Ctrl Pts',(0.116913659442519,0.100696009035903,
0.256079204996931));
#18570=CARTESIAN_POINT('Ctrl Pts',(0.149644807637716,0.0626933279972582,
0.253492546360598));
#18571=CARTESIAN_POINT('Ctrl Pts',(0.174757532207842,-0.0470233419515556,
0.248319229087933));
#18572=CARTESIAN_POINT('Ctrl Pts',(0.0589061664806588,-0.171273640229548,
0.240559253178935));
#18573=CARTESIAN_POINT('Ctrl Pts',(-0.108623733429488,-0.144737267461644,
0.232799277269938));
#18574=CARTESIAN_POINT('Ctrl Pts',(-0.180808275411966,0.00865192846140473,
0.225039301360939));
#18575=CARTESIAN_POINT('Ctrl Pts',(-0.0942515706791253,0.154556313135293,
0.217279325451942));
#18576=CARTESIAN_POINT('Ctrl Pts',(0.0750450248431312,0.164716481511431,
0.209519349542944));
#18577=CARTESIAN_POINT('Ctrl Pts',(0.178461260043253,0.0303012077178856,
0.201759373633945));
#18578=CARTESIAN_POINT('Ctrl Pts',(0.125203781387627,-0.130731709675357,
0.193999397724948));
#18579=CARTESIAN_POINT('Ctrl Pts',(-0.0379704533096903,-0.17698585337688,
0.18623942181595));
#18580=CARTESIAN_POINT('Ctrl Pts',(-0.167810456277154,-0.0678671379413016,
0.178479445906952));
#18581=CARTESIAN_POINT('Ctrl Pts',(-0.150328180300649,0.100834978066992,
0.170719469997954));
#18582=CARTESIAN_POINT('Ctrl Pts',(-0.000871711368246156,0.181012066871201,
0.162959494088956));
#18583=CARTESIAN_POINT('Ctrl Pts',(0.149350085565286,0.102277888352765,
0.155199518179958));
#18584=CARTESIAN_POINT('Ctrl Pts',(0.168456255263351,-0.0662471829332422,
0.14743954227096));
#18585=CARTESIAN_POINT('Ctrl Pts',(0.0396733728729688,-0.17661315503135,
0.139679566361963));
#18586=CARTESIAN_POINT('Ctrl Pts',(-0.123939070884463,-0.131929162812062,
0.131919590452964));
#18587=CARTESIAN_POINT('Ctrl Pts',(-0.178744451066417,0.0285765376657333,
0.124159614543967));
#18588=CARTESIAN_POINT('Ctrl Pts',(-0.0766286530280003,0.163994611436961,
0.116399638634969));
#18589=CARTESIAN_POINT('Ctrl Pts',(0.0927599764682439,0.155440618724813,
0.108639662725971));
#18590=CARTESIAN_POINT('Ctrl Pts',(0.180714016146597,0.0104239566588842,
0.100879686816973));
#18591=CARTESIAN_POINT('Ctrl Pts',(0.11001758793024,-0.143743725357685,
0.093119710907975));
#18592=CARTESIAN_POINT('Ctrl Pts',(-0.0572637123892103,-0.171718146500831,
0.0853597349989769));
#18593=CARTESIAN_POINT('Ctrl Pts',(-0.174273565575645,-0.048938961879483,
0.0775997590899791));
#18594=CARTESIAN_POINT('Ctrl Pts',(-0.138285748054726,0.11680239511684,
0.0698397831809812));
#18595=CARTESIAN_POINT('Ctrl Pts',(0.0191012565771036,0.180005302104073,
0.0620798072719832));
#18596=CARTESIAN_POINT('Ctrl Pts',(0.159724738700703,0.0851738948996701,
0.0543198313629854));
#18597=CARTESIAN_POINT('Ctrl Pts',(0.160113920417758,-0.0844204212478698,
0.0465598554539874));
#18598=CARTESIAN_POINT('Ctrl Pts',(0.0199582426985643,-0.179924098035372,
0.0387998795449896));
#18599=CARTESIAN_POINT('Ctrl Pts',(-0.137757819841364,-0.117427728395404,
0.0310399036359917));
#18600=CARTESIAN_POINT('Ctrl Pts',(-0.174460933778308,0.0480767578110765,
0.0232799277269937));
#18601=CARTESIAN_POINT('Ctrl Pts',(-0.0581466660421577,0.171532975008042,
0.0155199518179959));
#18602=CARTESIAN_POINT('Ctrl Pts',(0.109502662757235,0.144085240745689,
0.00775997590899784));
#18603=CARTESIAN_POINT('Ctrl Pts',(0.156737212705124,0.0419221657566679,
0.00258665863633264));
#18604=CARTESIAN_POINT('Ctrl Pts',(0.15408394018464,-0.00816268198427004,
0.));
#18605=CARTESIAN_POINT('Ctrl Pts',(0.15408394018464,-0.00816268198427004,
0.));
#18606=CARTESIAN_POINT('Ctrl Pts',(0.153697863146473,0.00250812953454787,
1.45220469349306E-17));
#18607=CARTESIAN_POINT('Ctrl Pts',(0.152123106309386,0.0130673133993916,
-2.32988231788825E-17));
#18608=CARTESIAN_POINT('Ctrl Pts',(0.149466152202855,0.0233620190894148,
-6.07153216591882E-17));
#18609=CARTESIAN_POINT('Ctrl Pts',(0.14793019248835,0.0293132898222067,
-8.23454409684948E-17));
#18610=CARTESIAN_POINT('Ctrl Pts',(0.146031563681721,0.0351760135160456,
3.17823908273165E-17));
#18611=CARTESIAN_POINT('Ctrl Pts',(0.143784059453749,0.0409171473780902,
6.24500451351651E-17));
#18612=CARTESIAN_POINT('Ctrl Pts',(0.142595904075608,0.0439522291322952,
7.86626679846993E-17));
#18613=CARTESIAN_POINT('Ctrl Pts',(0.141309213132582,0.0469553015723855,
1.03399090950918E-16));
#18614=CARTESIAN_POINT('Ctrl Pts',(0.13992871365498,0.0499144025840292,
1.00613961606655E-16));
#18615=CARTESIAN_POINT('Ctrl Pts',(0.135493978469587,0.0594202586791481,
9.16669744478229E-17));
#18616=CARTESIAN_POINT('Ctrl Pts',(0.130119641392827,0.0684241765595774,
5.76730757846686E-17));
#18617=CARTESIAN_POINT('Ctrl Pts',(0.123887660540245,0.0767683201192124,
1.38777878078145E-16));
#18618=CARTESIAN_POINT('Ctrl Pts',(0.120656388342022,0.0810947453345699,
1.808305895663E-16));
#18619=CARTESIAN_POINT('Ctrl Pts',(0.117193874983239,0.0852432898306738,
1.062697842984E-16));
#18620=CARTESIAN_POINT('Ctrl Pts',(0.11350808038867,0.0891875047540603,
1.14491749414469E-16));
#18621=CARTESIAN_POINT('Ctrl Pts',(0.110158526423333,0.0927719043720516,
1.21963656801269E-16));
#18622=CARTESIAN_POINT('Ctrl Pts',(0.106618991420749,0.0961915975683434,
1.17223950247179E-16));
#18623=CARTESIAN_POINT('Ctrl Pts',(0.102922970874274,0.0994011657423757,
1.02348685082632E-16));
#18624=CARTESIAN_POINT('Ctrl Pts',(0.0973787571548163,0.104215676830788,
8.00350512245867E-17));
#18625=CARTESIAN_POINT('Ctrl Pts',(0.0914754811895955,0.108568278221023,
6.56075743842472E-17));
#18626=CARTESIAN_POINT('Ctrl Pts',(0.0852365492443714,0.11239450959967,
3.29597460435593E-17));
#18627=CARTESIAN_POINT('Ctrl Pts',(0.0787787796913796,0.116354950379705,
-7.26807264206779E-19));
#18628=CARTESIAN_POINT('Ctrl Pts',(0.0719608771003193,0.11975150351845,
7.81983513604452E-17));
#18629=CARTESIAN_POINT('Ctrl Pts',(0.0648645680501024,0.122569786811788,
1.05818132034585E-16));
#18630=CARTESIAN_POINT('Ctrl Pts',(0.0619760396963809,0.123716959397427,
1.17060669392563E-16));
#18631=CARTESIAN_POINT('Ctrl Pts',(0.0590419697559043,0.124767587801255,
-1.70921410850511E-17));
#18632=CARTESIAN_POINT('Ctrl Pts',(0.0560804949635964,0.12571697313192,
-8.67361737988404E-19));
#18633=CARTESIAN_POINT('Ctrl Pts',(0.0481895916857994,0.128246627558523,
4.23638569993146E-17));
#18634=CARTESIAN_POINT('Ctrl Pts',(0.040081547172159,0.13006877931966,2.48189907303608E-17));
#18635=CARTESIAN_POINT('Ctrl Pts',(0.0318655688619291,0.131172622122806,
0.));
#18636=CARTESIAN_POINT('Ctrl Pts',(0.0267717292715239,0.131856995664207,
-1.5387571972871E-17));
#18637=CARTESIAN_POINT('Ctrl Pts',(0.0216363184326117,0.132264755542675,
5.61228976213782E-17));
#18638=CARTESIAN_POINT('Ctrl Pts',(0.0164863123329273,0.132388468809724,
3.03576608295941E-17));
#18639=CARTESIAN_POINT('Ctrl Pts',(0.0120733572364389,0.13249447666326,
8.27985532573229E-18));
#18640=CARTESIAN_POINT('Ctrl Pts',(0.00764667637530932,0.132391154756805,
7.9933444120104E-17));
#18641=CARTESIAN_POINT('Ctrl Pts',(0.00324855819595315,0.132074892239241,
9.62771529167128E-17));
#18642=CARTESIAN_POINT('Ctrl Pts',(-0.00215998367955725,0.131685971569047,
1.16375665467493E-16));
#18643=CARTESIAN_POINT('Ctrl Pts',(-0.00753310453775717,0.130975837616781,
1.12286849362194E-16));
#18644=CARTESIAN_POINT('Ctrl Pts',(-0.0128378223015392,0.129936202211006,
1.27068494615301E-16));
#18645=CARTESIAN_POINT('Ctrl Pts',(-0.0180922709275414,0.128906418710228,
1.41710064449709E-16));
#18646=CARTESIAN_POINT('Ctrl Pts',(-0.023283936630727,0.12755123862641,
1.19281234835921E-16));
#18647=CARTESIAN_POINT('Ctrl Pts',(-0.028350637156304,0.125868914531291,
9.19403442267708E-17));
#18648=CARTESIAN_POINT('Ctrl Pts',(-0.0326437071621008,0.124443463179602,
6.87741127091605E-17));
#18649=CARTESIAN_POINT('Ctrl Pts',(-0.0368509055758185,0.122782751372096,
3.08039683582783E-17));
#18650=CARTESIAN_POINT('Ctrl Pts',(-0.0409513668396969,0.120880349084932,
-1.95156391047391E-18));
#18651=CARTESIAN_POINT('Ctrl Pts',(-0.0436523616789034,0.119627226953286,
-2.45035827619675E-17));
#18652=CARTESIAN_POINT('Ctrl Pts',(-0.0463070048384274,0.118269169850402,
-4.56986185075063E-18));
#18653=CARTESIAN_POINT('Ctrl Pts',(-0.0489111879062984,0.116810626195002,
-1.73472347597681E-18));
#18654=CARTESIAN_POINT('Ctrl Pts',(0.0958116152722397,0.0825211298936481,
0.24));
#18655=CARTESIAN_POINT('Ctrl Pts',(0.102494250906434,0.0762804363331629,
0.24));
#18656=CARTESIAN_POINT('Ctrl Pts',(0.108399952301676,0.0693089192431419,
0.24));
#18657=CARTESIAN_POINT('Ctrl Pts',(0.113520383394708,0.0617855200816623,
0.24));
#18658=CARTESIAN_POINT('Ctrl Pts',(0.11760088593285,0.0557900777417299,
0.24));
#18659=CARTESIAN_POINT('Ctrl Pts',(0.1211824537664,0.0494427873910869,0.24));
#18660=CARTESIAN_POINT('Ctrl Pts',(0.124247292533427,0.0428169095598754,
0.24));
#18661=CARTESIAN_POINT('Ctrl Pts',(0.125635784531567,0.0398151273949318,
0.24));
#18662=CARTESIAN_POINT('Ctrl Pts',(0.126914357096627,0.0367636074968772,
0.24));
#18663=CARTESIAN_POINT('Ctrl Pts',(0.128080244072735,0.0336751552254939,
0.24));
#18664=CARTESIAN_POINT('Ctrl Pts',(0.13155694143068,0.024465331227027,0.24));
#18665=CARTESIAN_POINT('Ctrl Pts',(0.134041462136676,0.0149150332268467,
0.24));
#18666=CARTESIAN_POINT('Ctrl Pts',(0.135496608205084,0.00520422800883078,
0.24));
#18667=CARTESIAN_POINT('Ctrl Pts',(0.136052940597398,0.00149158663520877,
0.24));
#18668=CARTESIAN_POINT('Ctrl Pts',(0.136458356591543,-0.00224482315054724,
0.24));
#18669=CARTESIAN_POINT('Ctrl Pts',(0.136708928272429,-0.00599574054845843,
0.24));
#18670=CARTESIAN_POINT('Ctrl Pts',(0.136894600108428,-0.00877514370161729,
0.24));
#18671=CARTESIAN_POINT('Ctrl Pts',(0.136994942037659,-0.0115613689854128,
0.24));
#18672=CARTESIAN_POINT('Ctrl Pts',(0.137008733057845,-0.0143405417274864,
0.24));
#18673=CARTESIAN_POINT('Ctrl Pts',(0.137045731231951,-0.0217964308202384,
0.24));
#18674=CARTESIAN_POINT('Ctrl Pts',(0.136462408227525,-0.0292204075226799,
0.24));
#18675=CARTESIAN_POINT('Ctrl Pts',(0.135240454646173,-0.0365388974416549,
0.24));
#18676=CARTESIAN_POINT('Ctrl Pts',(0.134058793448489,-0.0436160693529878,
0.24));
#18677=CARTESIAN_POINT('Ctrl Pts',(0.132280018312676,-0.050595007513092,
0.24));
#18678=CARTESIAN_POINT('Ctrl Pts',(0.129952822193542,-0.0574290655609092,
0.24));
#18679=CARTESIAN_POINT('Ctrl Pts',(0.128850070284018,-0.0606674134165377,
0.24));
#18680=CARTESIAN_POINT('Ctrl Pts',(0.127623182384127,-0.0638741644409745,
0.24));
#18681=CARTESIAN_POINT('Ctrl Pts',(0.126284110088584,-0.067028198101918,
0.24));
#18682=CARTESIAN_POINT('Ctrl Pts',(0.122654675969015,-0.0755769205431157,
0.24));
#18683=CARTESIAN_POINT('Ctrl Pts',(0.118195290975453,-0.0837663478860722,
0.24));
#18684=CARTESIAN_POINT('Ctrl Pts',(0.113014989178579,-0.0915013065162071,
0.24));
#18685=CARTESIAN_POINT('Ctrl Pts',(0.108985931714537,-0.0975172866704144,
0.24));
#18686=CARTESIAN_POINT('Ctrl Pts',(0.104519884911976,-0.103258562704539,
0.24));
#18687=CARTESIAN_POINT('Ctrl Pts',(0.0996546828651377,-0.108675969178894,
0.24));
#18688=CARTESIAN_POINT('Ctrl Pts',(0.0972822643803542,-0.11131765910988,
0.24));
#18689=CARTESIAN_POINT('Ctrl Pts',(0.09482095240722,-0.113875293456495,
0.24));
#18690=CARTESIAN_POINT('Ctrl Pts',(0.0922773332174137,-0.116342466058553,
0.24));
#18691=CARTESIAN_POINT('Ctrl Pts',(0.0868426048671788,-0.121613857680014,
0.24));
#18692=CARTESIAN_POINT('Ctrl Pts',(0.0810310485854155,-0.126474759557936,
0.24));
#18693=CARTESIAN_POINT('Ctrl Pts',(0.0748870600798396,-0.130870957562724,
0.24));
#18694=CARTESIAN_POINT('Ctrl Pts',(0.0715378781224404,-0.133267392228159,
0.24));
#18695=CARTESIAN_POINT('Ctrl Pts',(0.0680912231566627,-0.135524142754832,
0.24));
#18696=CARTESIAN_POINT('Ctrl Pts',(0.0645638484115253,-0.13762659390894,
0.24));
#18697=CARTESIAN_POINT('Ctrl Pts',(0.0598451535113139,-0.140439117742,0.24));
#18698=CARTESIAN_POINT('Ctrl Pts',(0.0549775790306604,-0.142978967531553,
0.24));
#18699=CARTESIAN_POINT('Ctrl Pts',(0.0499773507040556,-0.145225083935062,
0.24));
#18700=CARTESIAN_POINT('Ctrl Pts',(0.0466920976074369,-0.146700828718701,
0.24));
#18701=CARTESIAN_POINT('Ctrl Pts',(0.0433495270099635,-0.148049731670784,
0.24));
#18702=CARTESIAN_POINT('Ctrl Pts',(0.039956549802796,-0.149273502906639,
0.24));
#18703=CARTESIAN_POINT('Ctrl Pts',(-0.126296536029262,-6.10717992316628E-5,
0.159341967361942));
#18704=CARTESIAN_POINT('Ctrl Pts',(-0.12637083907321,-0.0163056929409037,
0.160361391877968));
#18705=CARTESIAN_POINT('Ctrl Pts',(-0.12344809088261,-0.0325245895549842,
0.161380816393994));
#18706=CARTESIAN_POINT('Ctrl Pts',(-0.117399968681154,-0.0474794518833934,
0.162400240910021));
#18707=CARTESIAN_POINT('Ctrl Pts',(-0.102053636235694,-0.0854254922118417,
0.164986899546353));
#18708=CARTESIAN_POINT('Ctrl Pts',(-0.0665853528586453,-0.115233359066084,
0.167573558182686));
#18709=CARTESIAN_POINT('Ctrl Pts',(-0.0265641275910804,-0.123819689910512,
0.170160216819019));
#18710=CARTESIAN_POINT('Ctrl Pts',(0.0134570976764845,-0.13240602075494,
0.172746875455351));
#18711=CARTESIAN_POINT('Ctrl Pts',(0.058031264834566,-0.119770815589554,
0.175333534091684));
#18712=CARTESIAN_POINT('Ctrl Pts',(0.0875924985281064,-0.0914586003428122,
0.177920192728017));
#18713=CARTESIAN_POINT('Ctrl Pts',(0.117153732221647,-0.0631463850960709,
0.180506851364349));
#18714=CARTESIAN_POINT('Ctrl Pts',(0.131702032450646,-0.0191571597679751,
0.183093510000682));
#18715=CARTESIAN_POINT('Ctrl Pts',(0.124851119980295,0.0211965060081854,
0.185680168637015));
#18716=CARTESIAN_POINT('Ctrl Pts',(0.118000207509943,0.0615501717843459,
0.188266827273347));
#18717=CARTESIAN_POINT('Ctrl Pts',(0.0897500823402403,0.0982682780085711,
0.19085348590968));
#18718=CARTESIAN_POINT('Ctrl Pts',(0.0525017161220023,0.115239608835997,
0.193440144546013));
#18719=CARTESIAN_POINT('Ctrl Pts',(0.0152533499037644,0.132210939663423,
0.196026803182345));
#18720=CARTESIAN_POINT('Ctrl Pts',(-0.030993257363009,0.129435495094051,
0.198613461818678));
#18721=CARTESIAN_POINT('Ctrl Pts',(-0.0659388717692058,0.108119484364762,
0.20120012045501));
#18722=CARTESIAN_POINT('Ctrl Pts',(-0.100884486175403,0.0868034736354726,
0.203786779091343));
#18723=CARTESIAN_POINT('Ctrl Pts',(-0.124529107721023,0.0469468967462671,
0.206373437727676));
#18724=CARTESIAN_POINT('Ctrl Pts',(-0.126492123469331,0.00606801008988057,
0.208960096364008));
#18725=CARTESIAN_POINT('Ctrl Pts',(-0.126588724127832,0.00405634646811867,
0.209087386696653));
#18726=CARTESIAN_POINT('Ctrl Pts',(-0.126632819376787,0.00204220716288977,
0.209214677029297));
#18727=CARTESIAN_POINT('Ctrl Pts',(-0.126625441102054,2.7778768752873E-5,
0.209341967361942));
#18728=CARTESIAN_POINT('Ctrl Pts',(-0.0398513841857245,-0.149064942821851,
0.24));
#18729=CARTESIAN_POINT('Ctrl Pts',(-0.0883048112969314,-0.136111285829332,
0.237413341363667));
#18730=CARTESIAN_POINT('Ctrl Pts',(-0.170871437255804,-0.0596187094618861,
0.232240024091002));
#18731=CARTESIAN_POINT('Ctrl Pts',(-0.145169204726118,0.108307533342445,
0.224480048182004));
#18732=CARTESIAN_POINT('Ctrl Pts',(0.00818767200092134,0.180778621679153,
0.216720072273006));
#18733=CARTESIAN_POINT('Ctrl Pts',(0.154249898498561,0.0947283641859207,
0.208960096364008));
#18734=CARTESIAN_POINT('Ctrl Pts',(0.164950538597243,-0.0745810526211722,
0.201200120455011));
#18735=CARTESIAN_POINT('Ctrl Pts',(0.0308106631569891,-0.178364693496558,
0.193440144546012));
#18736=CARTESIAN_POINT('Ctrl Pts',(-0.13036283225522,-0.125587074703769,
0.185680168637015));
#18737=CARTESIAN_POINT('Ctrl Pts',(-0.17709781441264,0.03745832727601,0.177920192728017));
#18738=CARTESIAN_POINT('Ctrl Pts',(-0.0683530255288039,0.167611467503216,
0.170160216819019));
#18739=CARTESIAN_POINT('Ctrl Pts',(0.100397202365132,0.150621028353064,
0.162400240910021));
#18740=CARTESIAN_POINT('Ctrl Pts',(0.18100910679194,0.00139719974911195,
0.154640265001023));
#18741=CARTESIAN_POINT('Ctrl Pts',(0.102711092909207,-0.149052183789333,
0.146880289092025));
#18742=CARTESIAN_POINT('Ctrl Pts',(-0.0657574679958034,-0.168648048308422,
0.139120313183027));
#18743=CARTESIAN_POINT('Ctrl Pts',(-0.176497206835689,-0.0401861834345609,
0.131360337274029));
#18744=CARTESIAN_POINT('Ctrl Pts',(-0.132288575936487,0.123555290563421,
0.123600361365031));
#18745=CARTESIAN_POINT('Ctrl Pts',(0.0280571680938306,0.178826694862324,
0.115840385456033));
#18746=CARTESIAN_POINT('Ctrl Pts',(0.163771354656592,0.0771047007047774,
0.108080409547035));
#18747=CARTESIAN_POINT('Ctrl Pts',(0.155709331479018,-0.0923080778690166,
0.100320433638038));
#18748=CARTESIAN_POINT('Ctrl Pts',(0.0109489686262093,-0.180682908560435,
0.0925604577290397));
#18749=CARTESIAN_POINT('Ctrl Pts',(-0.143423754439364,-0.110434756566834,
0.0848004818200417));
#18750=CARTESIAN_POINT('Ctrl Pts',(-0.17188331593326,0.0567648465404429,
0.0770405059110439));
#18751=CARTESIAN_POINT('Ctrl Pts',(-0.0494457976037486,0.174130301808973,
0.0692805300020459));
#18752=CARTESIAN_POINT('Ctrl Pts',(0.11640175885633,0.13862511662766,0.061520554093048));
#18753=CARTESIAN_POINT('Ctrl Pts',(0.18005704388064,-0.0185795878987759,
0.0537605781840501));
#18754=CARTESIAN_POINT('Ctrl Pts',(0.0856431484406112,-0.159474177462153,
0.0460006022750521));
#18755=CARTESIAN_POINT('Ctrl Pts',(-0.0839657292871194,-0.160363143120653,
0.0382406263660544));
#18756=CARTESIAN_POINT('Ctrl Pts',(-0.179844832231877,-0.0204718628801216,
0.0304806504570563));
#18757=CARTESIAN_POINT('Ctrl Pts',(-0.117866479118068,0.137399078213474,
0.0227206745480585));
#18758=CARTESIAN_POINT('Ctrl Pts',(0.0476444145610997,0.174632482457551,
0.0149606986390605));
#18759=CARTESIAN_POINT('Ctrl Pts',(0.171219786572432,0.0585809927800803,
0.00720072273006264));
#18760=CARTESIAN_POINT('Ctrl Pts',(0.144688050375066,-0.108949473877577,
-0.000559253178935319));
#18761=CARTESIAN_POINT('Ctrl Pts',(-0.0092814439579932,-0.180735423716049,
-0.00831922908793317));
#18762=CARTESIAN_POINT('Ctrl Pts',(-0.105867686800049,-0.122947365648507,
-0.0134925463605985));
#18763=CARTESIAN_POINT('Ctrl Pts',(-0.131895903200816,-0.0800747195988904,
-0.0160792049969312));
#18764=CARTESIAN_POINT('Ctrl Pts',(-0.0374537582415196,-0.140096572423086,
0.245359734998977));
#18765=CARTESIAN_POINT('Ctrl Pts',(-0.0829920245295529,-0.127922261611689,
0.242773076362644));
#18766=CARTESIAN_POINT('Ctrl Pts',(-0.160591096949962,-0.0560317985556137,
0.237599759089979));
#18767=CARTESIAN_POINT('Ctrl Pts',(-0.13643521822445,0.101791299158848,
0.229839783180981));
#18768=CARTESIAN_POINT('Ctrl Pts',(0.00769506740980954,0.1699022237233,
0.222079807271983));
#18769=CARTESIAN_POINT('Ctrl Pts',(0.144969579481095,0.0890291096113304,
0.214319831362985));
#18770=CARTESIAN_POINT('Ctrl Pts',(0.155026424317845,-0.0700939445729984,
0.206559855453987));
#18771=CARTESIAN_POINT('Ctrl Pts',(0.0289569648011409,-0.167633527556011,
0.19879987954499));
#18772=CARTESIAN_POINT('Ctrl Pts',(-0.122519659046519,-0.118031231043151,
0.191039903635991));
#18773=CARTESIAN_POINT('Ctrl Pts',(-0.166442869216287,0.0352046776440443,
0.183279927726994));
#18774=CARTESIAN_POINT('Ctrl Pts',(-0.064240621638164,0.157527260611955,
0.175519951817996));
#18775=CARTESIAN_POINT('Ctrl Pts',(0.0943568867767351,0.141559037340679,
0.167759975908998));
#18776=CARTESIAN_POINT('Ctrl Pts',(0.170118841887737,0.00131313836865665,
0.16));
#18777=CARTESIAN_POINT('Ctrl Pts',(0.0965315639882279,-0.140084581027326,
0.152240024091002));
#18778=CARTESIAN_POINT('Ctrl Pts',(-0.0618012237018238,-0.158501476380598,
0.144480048182004));
#18779=CARTESIAN_POINT('Ctrl Pts',(-0.165878396703103,-0.0377684145673052,
0.136720072273006));
#18780=CARTESIAN_POINT('Ctrl Pts',(-0.124329541933827,0.116121687534276,
0.128960096364008));
#18781=CARTESIAN_POINT('Ctrl Pts',(0.0263691315170036,0.168067732987372,
0.12120012045501));
#18782=CARTESIAN_POINT('Ctrl Pts',(0.153918185014798,0.0724657594331675,
0.113440144546012));
#18783=CARTESIAN_POINT('Ctrl Pts',(0.146341206869619,-0.0867544378416841,
0.105680168637015));
#18784=CARTESIAN_POINT('Ctrl Pts',(0.0102902328814698,-0.169812269106107,
0.0979201927280167));
#18785=CARTESIAN_POINT('Ctrl Pts',(-0.134794781526993,-0.103790539737311,
0.0901602168190187));
#18786=CARTESIAN_POINT('Ctrl Pts',(-0.161542096774173,0.0533496359633175,
0.0824002409100209));
#18787=CARTESIAN_POINT('Ctrl Pts',(-0.0464709316213242,0.163653894581969,
0.074640265001023));
#18788=CARTESIAN_POINT('Ctrl Pts',(0.109398542213106,0.130284849835523,
0.066880289092025));
#18789=CARTESIAN_POINT('Ctrl Pts',(0.16922405906302,-0.0174617621848401,
0.0591203131830272));
#18790=CARTESIAN_POINT('Ctrl Pts',(0.0804904984426183,-0.149879543972585,
0.0513603372740291));
#18791=CARTESIAN_POINT('Ctrl Pts',(-0.0789139998409189,-0.150715025739123,
0.0436003613650314));
#18792=CARTESIAN_POINT('Ctrl Pts',(-0.169024614954586,-0.0192401899891918,
0.0358403854560333));
#18793=CARTESIAN_POINT('Ctrl Pts',(-0.110775138777956,0.12913257502003,
0.0280804095470356));
#18794=CARTESIAN_POINT('Ctrl Pts',(0.0447779273164969,0.164125861942445,
0.0203204336380375));
#18795=CARTESIAN_POINT('Ctrl Pts',(0.16091848811479,0.0550565152494576,
0.0125604577290397));
#18796=CARTESIAN_POINT('Ctrl Pts',(0.135983012131502,-0.10239461786658,
0.00480048182004171));
#18797=CARTESIAN_POINT('Ctrl Pts',(-0.00872303347143,-0.169861624730324,
-0.00295949408895612));
#18798=CARTESIAN_POINT('Ctrl Pts',(-0.0994982439886826,-0.115550337924785,
-0.00813281136162148));
#18799=CARTESIAN_POINT('Ctrl Pts',(-0.123960494032221,-0.0752570895690155,
-0.0107194699979541));
#18800=CARTESIAN_POINT('Ctrl Pts',(-0.0350561322973148,-0.13112820202432,
0.250719469997954));
#18801=CARTESIAN_POINT('Ctrl Pts',(-0.0776792377621743,-0.119733237394047,
0.248132811361621));
#18802=CARTESIAN_POINT('Ctrl Pts',(-0.150310756644121,-0.0524448876493412,
0.242959494088956));
#18803=CARTESIAN_POINT('Ctrl Pts',(-0.127701231722781,0.0952750649752511,
0.235199518179958));
#18804=CARTESIAN_POINT('Ctrl Pts',(0.00720246281869772,0.159025825767447,
0.22743954227096));
#18805=CARTESIAN_POINT('Ctrl Pts',(0.135689260463629,0.08332985503674,0.219679566361962));
#18806=CARTESIAN_POINT('Ctrl Pts',(0.145102310038447,-0.0656068365248246,
0.211919590452964));
#18807=CARTESIAN_POINT('Ctrl Pts',(0.0271032664452926,-0.156902361615465,
0.204159614543967));
#18808=CARTESIAN_POINT('Ctrl Pts',(-0.114676485837817,-0.110475387382534,
0.196399638634969));
#18809=CARTESIAN_POINT('Ctrl Pts',(-0.155787924019933,0.0329510280120788,
0.188639662725971));
#18810=CARTESIAN_POINT('Ctrl Pts',(-0.0601282177475243,0.147443053720694,
0.180879686816973));
#18811=CARTESIAN_POINT('Ctrl Pts',(0.0883165711883383,0.132497046328295,
0.173119710907975));
#18812=CARTESIAN_POINT('Ctrl Pts',(0.159228576983534,0.00122907698820117,
0.165359734998977));
#18813=CARTESIAN_POINT('Ctrl Pts',(0.0903520350672485,-0.131116978265319,
0.157599759089979));
#18814=CARTESIAN_POINT('Ctrl Pts',(-0.0578449794078444,-0.148354904452775,
0.149839783180981));
#18815=CARTESIAN_POINT('Ctrl Pts',(-0.155259586570517,-0.0353506457000499,
0.142079807271983));
#18816=CARTESIAN_POINT('Ctrl Pts',(-0.116370507931168,0.108688084505131,
0.134319831362985));
#18817=CARTESIAN_POINT('Ctrl Pts',(0.0246810949401768,0.157308771112418,
0.126559855453988));
#18818=CARTESIAN_POINT('Ctrl Pts',(0.144065015373005,0.0678268181615582,
0.118799879544989));
#18819=CARTESIAN_POINT('Ctrl Pts',(0.13697308226022,-0.0812007978143519,
0.111039903635992));
#18820=CARTESIAN_POINT('Ctrl Pts',(0.00963149713673027,-0.15894162965178,
0.103279927726994));
#18821=CARTESIAN_POINT('Ctrl Pts',(-0.126165808614623,-0.0971463229077874,
0.0955199518179957));
#18822=CARTESIAN_POINT('Ctrl Pts',(-0.151200877615086,0.0499344253861922,
0.087759975908998));
#18823=CARTESIAN_POINT('Ctrl Pts',(-0.0434960656388994,0.153177487354966,
0.08));
#18824=CARTESIAN_POINT('Ctrl Pts',(0.102395325569881,0.121944583043386,
0.072240024091002));
#18825=CARTESIAN_POINT('Ctrl Pts',(0.158391074245402,-0.0163439364709043,
0.0644800481820042));
#18826=CARTESIAN_POINT('Ctrl Pts',(0.0753378484446251,-0.140284910483017,
0.0567200722730062));
#18827=CARTESIAN_POINT('Ctrl Pts',(-0.0738622703947183,-0.141066908357593,
0.0489600963640083));
#18828=CARTESIAN_POINT('Ctrl Pts',(-0.158204397677296,-0.018008517098262,
0.0412001204550104));
#18829=CARTESIAN_POINT('Ctrl Pts',(-0.103683798437843,0.120866071826586,
0.0334401445460125));
#18830=CARTESIAN_POINT('Ctrl Pts',(0.0419114400718942,0.153619241427338,
0.0256801686370146));
#18831=CARTESIAN_POINT('Ctrl Pts',(0.150617189657149,0.051532037718835,
0.0179201927280167));
#18832=CARTESIAN_POINT('Ctrl Pts',(0.127277973887939,-0.0958397618555833,
0.0101602168190187));
#18833=CARTESIAN_POINT('Ctrl Pts',(-0.00816462298486686,-0.1589878257446,
0.00240024091002091));
#18834=CARTESIAN_POINT('Ctrl Pts',(-0.0931288011773165,-0.108153310201063,
-0.00277307636264444));
#18835=CARTESIAN_POINT('Ctrl Pts',(-0.116025084863626,-0.0704394595391406,
-0.00535973499897709));
#18836=CARTESIAN_POINT('Ctrl Pts',(-0.0326585063531099,-0.122159831625555,
0.256079204996931));
#18837=CARTESIAN_POINT('Ctrl Pts',(-0.0723664509947957,-0.111544213176404,
0.253492546360598));
#18838=CARTESIAN_POINT('Ctrl Pts',(-0.140030416338279,-0.0488579767430688,
0.248319229087933));
#18839=CARTESIAN_POINT('Ctrl Pts',(-0.118967245221113,0.0887588307916541,
0.240559253178936));
#18840=CARTESIAN_POINT('Ctrl Pts',(0.00670985822758596,0.148149427811594,
0.232799277269937));
#18841=CARTESIAN_POINT('Ctrl Pts',(0.126408941446163,0.0776306004621497,
0.225039301360939));
#18842=CARTESIAN_POINT('Ctrl Pts',(0.13517819575905,-0.0611197284766509,
0.217279325451942));
#18843=CARTESIAN_POINT('Ctrl Pts',(0.0252495680894444,-0.146171195674918,
0.209519349542944));
#18844=CARTESIAN_POINT('Ctrl Pts',(-0.106833312629116,-0.102919543721916,
0.201759373633946));
#18845=CARTESIAN_POINT('Ctrl Pts',(-0.14513297882358,0.0306973783801131,
0.193999397724948));
#18846=CARTESIAN_POINT('Ctrl Pts',(-0.0560158138568844,0.137358846829434,
0.18623942181595));
#18847=CARTESIAN_POINT('Ctrl Pts',(0.0822762555999414,0.12343505531591,
0.178479445906952));
#18848=CARTESIAN_POINT('Ctrl Pts',(0.148338312079331,0.00114501560774606,
0.170719469997954));
#18849=CARTESIAN_POINT('Ctrl Pts',(0.0841725061462688,-0.122149375503312,
0.162959494088956));
#18850=CARTESIAN_POINT('Ctrl Pts',(-0.0538887351138648,-0.138208332524951,
0.155199518179959));
#18851=CARTESIAN_POINT('Ctrl Pts',(-0.144640776437932,-0.0329328768327946,
0.14743954227096));
#18852=CARTESIAN_POINT('Ctrl Pts',(-0.108411473928508,0.101254481475986,
0.139679566361963));
#18853=CARTESIAN_POINT('Ctrl Pts',(0.0229930583633497,0.146549809237466,
0.131919590452964));
#18854=CARTESIAN_POINT('Ctrl Pts',(0.134211845731212,0.0631878768899486,
0.124159614543967));
#18855=CARTESIAN_POINT('Ctrl Pts',(0.127604957650822,-0.0756471577870196,
0.116399638634969));
#18856=CARTESIAN_POINT('Ctrl Pts',(0.00897276139199077,-0.148070990197453,
0.108639662725971));
#18857=CARTESIAN_POINT('Ctrl Pts',(-0.117536835702253,-0.0905021060782641,
0.100879686816973));
#18858=CARTESIAN_POINT('Ctrl Pts',(-0.140859658455999,0.0465192148090667,
0.0931197109079749));
#18859=CARTESIAN_POINT('Ctrl Pts',(-0.0405211996564747,0.142701080127962,
0.0853597349989771));
#18860=CARTESIAN_POINT('Ctrl Pts',(0.0953921089266558,0.113604316251249,
0.077599759089979));
#18861=CARTESIAN_POINT('Ctrl Pts',(0.147558089427783,-0.0152261107569683,
0.0698397831809813));
#18862=CARTESIAN_POINT('Ctrl Pts',(0.070185198446632,-0.130690276993449,
0.0620798072719832));
#18863=CARTESIAN_POINT('Ctrl Pts',(-0.0688105409485176,-0.131418790976063,
0.0543198313629854));
#18864=CARTESIAN_POINT('Ctrl Pts',(-0.147384180400005,-0.0167768442073323,
0.0465598554539874));
#18865=CARTESIAN_POINT('Ctrl Pts',(-0.0965924580977301,0.112599568633142,
0.0387998795449896));
#18866=CARTESIAN_POINT('Ctrl Pts',(0.0390449528272914,0.143112620912232,
0.0310399036359916));
#18867=CARTESIAN_POINT('Ctrl Pts',(0.140315891199508,0.0480075601882123,
0.0232799277269937));
#18868=CARTESIAN_POINT('Ctrl Pts',(0.118572935644375,-0.0892849058445864,
0.0155199518179958));
#18869=CARTESIAN_POINT('Ctrl Pts',(-0.00760621249830358,-0.148114026758875,
0.00775997590899793));
#18870=CARTESIAN_POINT('Ctrl Pts',(-0.0867593583659504,-0.100756282477341,
0.00258665863633259));
#18871=CARTESIAN_POINT('Ctrl Pts',(-0.108089675695031,-0.0656218295092657,
-5.55111512312578E-17));
#18872=CARTESIAN_POINT('Ctrl Pts',(-0.108089675695031,-0.0656218295092657,
-5.55111512312578E-17));
#18873=CARTESIAN_POINT('Ctrl Pts',(-0.104219465379748,-0.0739058869203245,
-4.02841154597017E-17));
#18874=CARTESIAN_POINT('Ctrl Pts',(-0.0994141168358061,-0.0816768736924768,
-5.16144647363644E-17));
#18875=CARTESIAN_POINT('Ctrl Pts',(-0.0938412360364922,-0.088871564406415,
-3.81639164714898E-17));
#18876=CARTESIAN_POINT('Ctrl Pts',(-0.0894001862863345,-0.094605040600905,
-2.74451237748006E-17));
#18877=CARTESIAN_POINT('Ctrl Pts',(-0.0844703330957707,-0.0999727304469881,
3.12377098840079E-17));
#18878=CARTESIAN_POINT('Ctrl Pts',(-0.0791158513129458,-0.104935071387697,
-1.21430643318376E-17));
#18879=CARTESIAN_POINT('Ctrl Pts',(-0.0766900604813501,-0.107183206995485,
-3.17962611543325E-17));
#18880=CARTESIAN_POINT('Ctrl Pts',(-0.0741829996358932,-0.109342173006691,
4.83248416902999E-17));
#18881=CARTESIAN_POINT('Ctrl Pts',(-0.0716059924168524,-0.111405381598006,
5.3776427755281E-17));
#18882=CARTESIAN_POINT('Ctrl Pts',(-0.0639212992135713,-0.117557915794061,
7.00331794132204E-17));
#18883=CARTESIAN_POINT('Ctrl Pts',(-0.0556061968393146,-0.12287204611112,
-5.69073736333764E-18));
#18884=CARTESIAN_POINT('Ctrl Pts',(-0.0468203466856493,-0.127256781127915,
5.55111512312578E-17));
#18885=CARTESIAN_POINT('Ctrl Pts',(-0.0434613267337519,-0.12893315986732,
7.89099528597243E-17));
#18886=CARTESIAN_POINT('Ctrl Pts',(-0.0400330653128497,-0.130473352587733,
3.97002991909352E-17));
#18887=CARTESIAN_POINT('Ctrl Pts',(-0.0365431560942257,-0.131870761756357,
6.59194920871187E-17));
#18888=CARTESIAN_POINT('Ctrl Pts',(-0.0339571636773035,-0.13290622981212,
8.5347686277821E-17));
#18889=CARTESIAN_POINT('Ctrl Pts',(-0.0313383144727484,-0.133862652235137,
-2.74403076010104E-17));
#18890=CARTESIAN_POINT('Ctrl Pts',(-0.0286994266230122,-0.134734580282325,
-2.42861286636753E-17));
#18891=CARTESIAN_POINT('Ctrl Pts',(-0.0216199050576346,-0.137073760181214,
-1.58242011095522E-17));
#18892=CARTESIAN_POINT('Ctrl Pts',(-0.0143790427459088,-0.138813119073991,
5.80198461902811E-17));
#18893=CARTESIAN_POINT('Ctrl Pts',(-0.0070411538297537,-0.139912507657099,
6.93889390390723E-17));
#18894=CARTESIAN_POINT('Ctrl Pts',(5.47883476400097E-5,-0.140975646920361,
8.02325614020808E-17));
#18895=CARTESIAN_POINT('Ctrl Pts',(0.00724182591717642,-0.141440539972256,
1.32011341321413E-16));
#18896=CARTESIAN_POINT('Ctrl Pts',(0.0144605478337719,-0.141339082434075,
1.61329283265843E-16));
#18897=CARTESIAN_POINT('Ctrl Pts',(0.0178811722145177,-0.141291006315792,
1.75221724083914E-16));
#18898=CARTESIAN_POINT('Ctrl Pts',(0.021310106848269,-0.141115105569205,
1.85534911235541E-16));
#18899=CARTESIAN_POINT('Ctrl Pts',(0.0247235715439624,-0.140816220288761,
1.71737624121704E-16));
#18900=CARTESIAN_POINT('Ctrl Pts',(0.0339754553361668,-0.140006119078294,
1.34341339582434E-16));
#18901=CARTESIAN_POINT('Ctrl Pts',(0.0431421008898472,-0.138295657968001,
8.04496487960062E-17));
#18902=CARTESIAN_POINT('Ctrl Pts',(0.0520992976556894,-0.135759125106636,
3.20923843055709E-17));
#18903=CARTESIAN_POINT('Ctrl Pts',(0.0590658916121619,-0.13378629867842,
-5.518202506064E-18));
#18904=CARTESIAN_POINT('Ctrl Pts',(0.0659062642374416,-0.131312982137409,
7.87850579480063E-17));
#18905=CARTESIAN_POINT('Ctrl Pts',(0.0725619642951071,-0.128359965266718,
7.63278329429795E-17));
#18906=CARTESIAN_POINT('Ctrl Pts',(0.0758074813473741,-0.126919986522721,
7.51296170399226E-17));
#18907=CARTESIAN_POINT('Ctrl Pts',(0.0790005264283722,-0.125369490597537,
8.38688896655138E-17));
#18908=CARTESIAN_POINT('Ctrl Pts',(0.0821329715644795,-0.123712761836801,
7.24247051220317E-17));
#18909=CARTESIAN_POINT('Ctrl Pts',(0.0888257654942848,-0.120172989003949,
4.79730178566093E-17));
#18910=CARTESIAN_POINT('Ctrl Pts',(0.0952446087626691,-0.116147988031934,
8.96774285244103E-17));
#18911=CARTESIAN_POINT('Ctrl Pts',(0.101324221742587,-0.111663228753314,
8.28330459778925E-17));
#18912=CARTESIAN_POINT('Ctrl Pts',(0.104638321741973,-0.109218510516871,
7.91020571356516E-17));
#18913=CARTESIAN_POINT('Ctrl Pts',(0.107849695272814,-0.106637925639498,
3.17151869302413E-17));
#18914=CARTESIAN_POINT('Ctrl Pts',(0.110939265073957,-0.10393289123317,
1.53956708492942E-17));
#18915=CARTESIAN_POINT('Ctrl Pts',(0.115072333360666,-0.100314234708527,
-6.43574216607592E-18));
#18916=CARTESIAN_POINT('Ctrl Pts',(0.118992075260627,-0.0964697210975667,
5.54296751400654E-17));
#18917=CARTESIAN_POINT('Ctrl Pts',(0.122673447199167,-0.0924082746861152,
3.52365706057789E-17));
#18918=CARTESIAN_POINT('Ctrl Pts',(0.125092164655522,-0.0897398425098966,
2.31620156359627E-17));
#18919=CARTESIAN_POINT('Ctrl Pts',(0.127407959881093,-0.0869777021544565,
-4.01489640485901E-17));
#18920=CARTESIAN_POINT('Ctrl Pts',(0.129620323775263,-0.0841289546921697,
-3.98986399474666E-17));
#18921=CARTESIAN_POINT('Ctrl Pts',(-0.126471935391749,0.000101176582396995,
0.195658032638058));
#18922=CARTESIAN_POINT('Ctrl Pts',(-0.126547267107008,0.00888033934128026,
0.195105154333688));
#18923=CARTESIAN_POINT('Ctrl Pts',(-0.125707148272093,0.0176451944231377,
0.194552276029318));
#18924=CARTESIAN_POINT('Ctrl Pts',(-0.12389684029672,0.0262048027713284,
0.193999397724948));
#18925=CARTESIAN_POINT('Ctrl Pts',(-0.115427257168015,0.0662512011965534,
0.191412739088615));
#18926=CARTESIAN_POINT('Ctrl Pts',(-0.0857215355124495,0.101805024012994,
0.188826080452282));
#18927=CARTESIAN_POINT('Ctrl Pts',(-0.0478199964418627,0.117261303502293,
0.18623942181595));
#18928=CARTESIAN_POINT('Ctrl Pts',(-0.0099184573712758,0.132717582991593,
0.183652763179617));
#18929=CARTESIAN_POINT('Ctrl Pts',(0.0361788991143328,0.128076319153751,
0.181066104543285));
#18930=CARTESIAN_POINT('Ctrl Pts',(0.070237920103702,0.105374013950137,
0.178479445906952));
#18931=CARTESIAN_POINT('Ctrl Pts',(0.104296941093071,0.0826717087465222,
0.175892787270619));
#18932=CARTESIAN_POINT('Ctrl Pts',(0.126317626586201,0.0419083621771342,
0.173306128634287));
#18933=CARTESIAN_POINT('Ctrl Pts',(0.126633668343922,0.000977623707263797,
0.170719469997954));
#18934=CARTESIAN_POINT('Ctrl Pts',(0.126949710101644,-0.0399531147626067,
0.168132811361621));
#18935=CARTESIAN_POINT('Ctrl Pts',(0.105561108123956,-0.08105124513296,
0.165546152725289));
#18936=CARTESIAN_POINT('Ctrl Pts',(0.0718566002584231,-0.104276803155076,
0.162959494088956));
#18937=CARTESIAN_POINT('Ctrl Pts',(0.0381520923928904,-0.127502361177192,
0.160372835452623));
#18938=CARTESIAN_POINT('Ctrl Pts',(-0.00786832136048696,-0.132855346851071,
0.157786176816291));
#18939=CARTESIAN_POINT('Ctrl Pts',(-0.0460038684578537,-0.117985930405985,
0.155199518179958));
#18940=CARTESIAN_POINT('Ctrl Pts',(-0.0841394155552204,-0.103116513960899,
0.152612859543626));
#18941=CARTESIAN_POINT('Ctrl Pts',(-0.114390095996576,-0.0680246953968468,
0.150026200907293));
#18942=CARTESIAN_POINT('Ctrl Pts',(-0.12347721913235,-0.0281142263966907,
0.14743954227096));
#18943=CARTESIAN_POINT('Ctrl Pts',(-0.125563410841138,-0.018951712774069,
0.14684570572666));
#18944=CARTESIAN_POINT('Ctrl Pts',(-0.126534167537385,-0.00953522996602069,
0.146251869182359));
#18945=CARTESIAN_POINT('Ctrl Pts',(-0.126453631260982,-0.000102348163238207,
0.145658032638058));
#18946=CARTESIAN_POINT('Ctrl Pts',(-0.0398513841857245,-0.149064942821851,
0.24));
#18947=CARTESIAN_POINT('Ctrl Pts',(-0.0498806325786677,-0.145400296738327,
0.24));
#18948=CARTESIAN_POINT('Ctrl Pts',(-0.0594363948008725,-0.140639648297949,
0.24));
#18949=CARTESIAN_POINT('Ctrl Pts',(-0.0684062055177017,-0.134931499399492,
0.24));
#18950=CARTESIAN_POINT('Ctrl Pts',(-0.0735915624001909,-0.131631676235849,
0.24));
#18951=CARTESIAN_POINT('Ctrl Pts',(-0.0785806353345173,-0.128014298080738,
0.24));
#18952=CARTESIAN_POINT('Ctrl Pts',(-0.0833462611484583,-0.124102693747304,
0.24));
#18953=CARTESIAN_POINT('Ctrl Pts',(-0.0858656342542594,-0.122034803580736,
0.24));
#18954=CARTESIAN_POINT('Ctrl Pts',(-0.0883241156266364,-0.11988309220465,
0.24));
#18955=CARTESIAN_POINT('Ctrl Pts',(-0.0907117892851122,-0.117655751751618,
0.24));
#18956=CARTESIAN_POINT('Ctrl Pts',(-0.0983819858496404,-0.110500611839494,
0.24));
#18957=CARTESIAN_POINT('Ctrl Pts',(-0.105284458416918,-0.102606966330569,
0.24));
#18958=CARTESIAN_POINT('Ctrl Pts',(-0.111294422020379,-0.0941015332659665,
0.24));
#18959=CARTESIAN_POINT('Ctrl Pts',(-0.114410577497229,-0.0896914812962706,
0.24));
#18960=CARTESIAN_POINT('Ctrl Pts',(-0.117286101138547,-0.0851164738413172,
0.24));
#18961=CARTESIAN_POINT('Ctrl Pts',(-0.119898298320422,-0.0803922539627851,
0.24));
#18962=CARTESIAN_POINT('Ctrl Pts',(-0.1222721977331,-0.0760990011896685,
0.24));
#18963=CARTESIAN_POINT('Ctrl Pts',(-0.124430744329062,-0.0716759619599862,
0.24));
#18964=CARTESIAN_POINT('Ctrl Pts',(-0.126341093034125,-0.0671690272221462,
0.24));
#18965=CARTESIAN_POINT('Ctrl Pts',(-0.129206708925078,-0.060408406100978,
0.24));
#18966=CARTESIAN_POINT('Ctrl Pts',(-0.131522065955468,-0.0534490321795157,
0.24));
#18967=CARTESIAN_POINT('Ctrl Pts',(-0.133233091500091,-0.0463330844490581,
0.24));
#18968=CARTESIAN_POINT('Ctrl Pts',(-0.135004134506116,-0.0389675313754268,
0.24));
#18969=CARTESIAN_POINT('Ctrl Pts',(-0.136127599829873,-0.0314337185245799,
0.24));
#18970=CARTESIAN_POINT('Ctrl Pts',(-0.136615064298196,-0.0238138180582873,
0.24));
#18971=CARTESIAN_POINT('Ctrl Pts',(-0.136813484749433,-0.0207121682209076,
0.24));
#18972=CARTESIAN_POINT('Ctrl Pts',(-0.136906013213758,-0.0175970392000076,
0.24));
#18973=CARTESIAN_POINT('Ctrl Pts',(-0.136893785357156,-0.0144871321155608,
0.24));
#18974=CARTESIAN_POINT('Ctrl Pts',(-0.136861203984761,-0.00620072149302863,
0.24));
#18975=CARTESIAN_POINT('Ctrl Pts',(-0.136088646936857,0.00207357465703332,
0.24));
#18976=CARTESIAN_POINT('Ctrl Pts',(-0.134599584032292,0.0102285531249486,
0.24));
#18977=CARTESIAN_POINT('Ctrl Pts',(-0.133676409755049,0.0152843948425598,
0.24));
#18978=CARTESIAN_POINT('Ctrl Pts',(-0.132477333465274,0.0202942984003417,
0.24));
#18979=CARTESIAN_POINT('Ctrl Pts',(-0.131003622030167,0.0252303138624672,
0.24));
#18980=CARTESIAN_POINT('Ctrl Pts',(-0.129740734874544,0.029460199292259,
0.24));
#18981=CARTESIAN_POINT('Ctrl Pts',(-0.128274507607502,0.0336384499732856,
0.24));
#18982=CARTESIAN_POINT('Ctrl Pts',(-0.126614574688298,0.0377237273426867,
0.24));
#18983=CARTESIAN_POINT('Ctrl Pts',(-0.124573382985647,0.042747324485064,
0.24));
#18984=CARTESIAN_POINT('Ctrl Pts',(-0.122237651925267,0.0476379767326878,
0.24));
#18985=CARTESIAN_POINT('Ctrl Pts',(-0.119609691052418,0.0523617558795304,
0.24));
#18986=CARTESIAN_POINT('Ctrl Pts',(-0.117006563775536,0.0570408964535612,
0.24));
#18987=CARTESIAN_POINT('Ctrl Pts',(-0.114113358229268,0.0615597689541448,
0.24));
#18988=CARTESIAN_POINT('Ctrl Pts',(-0.110947628485839,0.0658586917144141,
0.24));
#18989=CARTESIAN_POINT('Ctrl Pts',(-0.108265305855902,0.0695011687224882,
0.24));
#18990=CARTESIAN_POINT('Ctrl Pts',(-0.105385772272888,0.0729892759232728,
0.24));
#18991=CARTESIAN_POINT('Ctrl Pts',(-0.102309360287629,0.0763011815833395,
0.24));
#18992=CARTESIAN_POINT('Ctrl Pts',(-0.100282916666232,0.0784827457339379,
0.24));
#18993=CARTESIAN_POINT('Ctrl Pts',(-0.0981709975111385,0.0805877996091198,
0.24));
#18994=CARTESIAN_POINT('Ctrl Pts',(-0.0959791030802606,0.0826138105732947,
0.24));
#18995=CARTESIAN_POINT('Origin',(0.,0.,0.24));
#18996=CARTESIAN_POINT('',(0.158771324027147,-0.275,0.24));
#18997=CARTESIAN_POINT('',(0.317542648054294,0.,0.24));
#18998=CARTESIAN_POINT('',(0.158771324027147,-0.275,0.24));
#18999=CARTESIAN_POINT('',(0.158771324027147,0.275,0.24));
#19000=CARTESIAN_POINT('',(0.317542648054294,0.,0.24));
#19001=CARTESIAN_POINT('',(-0.158771324027147,0.275,0.24));
#19002=CARTESIAN_POINT('',(0.158771324027147,0.275,0.24));
#19003=CARTESIAN_POINT('',(-0.317542648054294,5.55111512312578E-17,0.24));
#19004=CARTESIAN_POINT('',(-0.158771324027147,0.275,0.24));
#19005=CARTESIAN_POINT('',(-0.158771324027147,-0.275,0.24));
#19006=CARTESIAN_POINT('',(-0.317542648054294,3.88877587532466E-17,0.24));
#19007=CARTESIAN_POINT('',(-0.158771324027147,-0.275,0.24));
#19008=CARTESIAN_POINT('Origin',(0.,0.,0.12));
#19009=CARTESIAN_POINT('Origin',(-0.158771324027147,-0.275,0.));
#19010=CARTESIAN_POINT('',(-0.158771324027147,-0.275,0.));
#19011=CARTESIAN_POINT('',(0.158771324027147,-0.275,0.));
#19012=CARTESIAN_POINT('',(-0.158771324027147,-0.275,0.));
#19013=CARTESIAN_POINT('',(0.158771324027147,-0.275,0.));
#19014=CARTESIAN_POINT('',(-0.158771324027147,-0.275,0.));
#19015=CARTESIAN_POINT('Origin',(-0.317542648054294,3.88877587532466E-17,
0.));
#19016=CARTESIAN_POINT('',(-0.317542648054294,3.88877587532466E-17,0.));
#19017=CARTESIAN_POINT('',(-0.317542648054294,3.88877587532466E-17,0.));
#19018=CARTESIAN_POINT('',(-0.317542648054294,3.88877587532466E-17,0.));
#19019=CARTESIAN_POINT('Origin',(-0.158771324027147,0.275,0.));
#19020=CARTESIAN_POINT('',(-0.158771324027147,0.275,0.));
#19021=CARTESIAN_POINT('',(-0.158771324027147,0.275,0.));
#19022=CARTESIAN_POINT('',(-0.158771324027147,0.275,0.));
#19023=CARTESIAN_POINT('Origin',(0.158771324027147,0.275,0.));
#19024=CARTESIAN_POINT('',(0.158771324027147,0.275,0.));
#19025=CARTESIAN_POINT('',(0.158771324027147,0.275,0.));
#19026=CARTESIAN_POINT('',(0.158771324027147,0.275,0.));
#19027=CARTESIAN_POINT('Origin',(0.317542648054294,0.,0.));
#19028=CARTESIAN_POINT('',(0.317542648054294,0.,0.));
#19029=CARTESIAN_POINT('',(0.317542648054294,0.,0.));
#19030=CARTESIAN_POINT('',(0.317542648054294,0.,0.));
#19031=CARTESIAN_POINT('Origin',(0.158771324027147,-0.275,0.));
#19032=CARTESIAN_POINT('',(0.158771324027147,-0.275,0.));
#19033=CARTESIAN_POINT('Origin',(0.,0.,0.));
#19034=CARTESIAN_POINT('',(0.,0.,0.));
#19035=CARTESIAN_POINT('',(0.,0.,0.));
#19036=CARTESIAN_POINT('',(0.,0.,0.));
#19037=CARTESIAN_POINT('',(2.,0.,0.6));
#19038=CARTESIAN_POINT('',(2.,0.,-0.84));
#19039=CARTESIAN_POINT('',(0.,0.,0.));
#19040=CARTESIAN_POINT('',(11.2,0.,0.6));
#19041=CARTESIAN_POINT('',(11.2,0.,-0.84));
#19042=CARTESIAN_POINT('',(0.,0.,0.));
#19043=CARTESIAN_POINT('Origin',(0.,0.,0.));
#19044=CARTESIAN_POINT('',(-0.41,-5.02105187650415E-17,0.1));
#19045=CARTESIAN_POINT('Origin',(0.,0.,0.1));
#19046=CARTESIAN_POINT('',(-0.41,-5.02105187650415E-17,0.));
#19047=CARTESIAN_POINT('',(-0.41,-5.02105187650415E-17,0.));
#19048=CARTESIAN_POINT('Origin',(0.,0.,0.));
#19049=CARTESIAN_POINT('Origin',(0.,0.,0.));
#19050=CARTESIAN_POINT('',(-0.6,-7.34788079488412E-17,0.1));
#19051=CARTESIAN_POINT('Origin',(0.,0.,0.1));
#19052=CARTESIAN_POINT('',(-0.6,-7.34788079488412E-17,0.));
#19053=CARTESIAN_POINT('',(-0.6,-7.34788079488412E-17,0.));
#19054=CARTESIAN_POINT('Origin',(0.,0.,0.));
#19055=CARTESIAN_POINT('Origin',(0.,0.,0.1));
#19056=CARTESIAN_POINT('Origin',(0.,0.,0.));
#19057=CARTESIAN_POINT('',(0.,0.,0.));
#19058=CARTESIAN_POINT('',(0.,0.,0.));
#19059=CARTESIAN_POINT('',(4.,-2.5,0.3));
#19060=CARTESIAN_POINT('',(0.,0.,0.));
#19061=CARTESIAN_POINT('',(0.,0.,0.6));
#19062=CARTESIAN_POINT('',(0.,0.,0.7));
#19063=CARTESIAN_POINT('',(4.,2.5,-0.3));
#19064=CARTESIAN_POINT('',(0.,0.,-0.7));
#19065=UNCERTAINTY_MEASURE_WITH_UNIT(LENGTH_MEASURE(0.001),#19091,
'DISTANCE_ACCURACY_VALUE',
'Maximum model space distance between geometric entities at asserted c
onnectivities');
#19066=UNCERTAINTY_MEASURE_WITH_UNIT(LENGTH_MEASURE(0.001),#19091,
'DISTANCE_ACCURACY_VALUE',
'Maximum model space distance between geometric entities at asserted c
onnectivities');
#19067=UNCERTAINTY_MEASURE_WITH_UNIT(LENGTH_MEASURE(0.001),#19091,
'DISTANCE_ACCURACY_VALUE',
'Maximum model space distance between geometric entities at asserted c
onnectivities');
#19068=UNCERTAINTY_MEASURE_WITH_UNIT(LENGTH_MEASURE(0.001),#19091,
'DISTANCE_ACCURACY_VALUE',
'Maximum model space distance between geometric entities at asserted c
onnectivities');
#19069=UNCERTAINTY_MEASURE_WITH_UNIT(LENGTH_MEASURE(0.001),#19091,
'DISTANCE_ACCURACY_VALUE',
'Maximum model space distance between geometric entities at asserted c
onnectivities');
#19070=UNCERTAINTY_MEASURE_WITH_UNIT(LENGTH_MEASURE(0.001),#19091,
'DISTANCE_ACCURACY_VALUE',
'Maximum model space distance between geometric entities at asserted c
onnectivities');
#19071=UNCERTAINTY_MEASURE_WITH_UNIT(LENGTH_MEASURE(0.001),#19091,
'DISTANCE_ACCURACY_VALUE',
'Maximum model space distance between geometric entities at asserted c
onnectivities');
#19072=UNCERTAINTY_MEASURE_WITH_UNIT(LENGTH_MEASURE(0.001),#19091,
'DISTANCE_ACCURACY_VALUE',
'Maximum model space distance between geometric entities at asserted c
onnectivities');
#19073=UNCERTAINTY_MEASURE_WITH_UNIT(LENGTH_MEASURE(0.001),#19091,
'DISTANCE_ACCURACY_VALUE',
'Maximum model space distance between geometric entities at asserted c
onnectivities');
#19074=UNCERTAINTY_MEASURE_WITH_UNIT(LENGTH_MEASURE(0.001),#19091,
'DISTANCE_ACCURACY_VALUE',
'Maximum model space distance between geometric entities at asserted c
onnectivities');
#19075=UNCERTAINTY_MEASURE_WITH_UNIT(LENGTH_MEASURE(0.001),#19091,
'DISTANCE_ACCURACY_VALUE',
'Maximum model space distance between geometric entities at asserted c
onnectivities');
#19076=UNCERTAINTY_MEASURE_WITH_UNIT(LENGTH_MEASURE(0.001),#19091,
'DISTANCE_ACCURACY_VALUE',
'Maximum model space distance between geometric entities at asserted c
onnectivities');
#19077=UNCERTAINTY_MEASURE_WITH_UNIT(LENGTH_MEASURE(0.001),#19091,
'DISTANCE_ACCURACY_VALUE',
'Maximum model space distance between geometric entities at asserted c
onnectivities');
#19078=(
GEOMETRIC_REPRESENTATION_CONTEXT(3)
GLOBAL_UNCERTAINTY_ASSIGNED_CONTEXT((#19065))
GLOBAL_UNIT_ASSIGNED_CONTEXT((#19091,#19093,#19094))
REPRESENTATION_CONTEXT('','3D')
);
#19079=(
GEOMETRIC_REPRESENTATION_CONTEXT(3)
GLOBAL_UNCERTAINTY_ASSIGNED_CONTEXT((#19066))
GLOBAL_UNIT_ASSIGNED_CONTEXT((#19091,#19093,#19094))
REPRESENTATION_CONTEXT('','3D')
);
#19080=(
GEOMETRIC_REPRESENTATION_CONTEXT(3)
GLOBAL_UNCERTAINTY_ASSIGNED_CONTEXT((#19067))
GLOBAL_UNIT_ASSIGNED_CONTEXT((#19091,#19093,#19094))
REPRESENTATION_CONTEXT('','3D')
);
#19081=(
GEOMETRIC_REPRESENTATION_CONTEXT(3)
GLOBAL_UNCERTAINTY_ASSIGNED_CONTEXT((#19068))
GLOBAL_UNIT_ASSIGNED_CONTEXT((#19091,#19093,#19094))
REPRESENTATION_CONTEXT('','3D')
);
#19082=(
GEOMETRIC_REPRESENTATION_CONTEXT(3)
GLOBAL_UNCERTAINTY_ASSIGNED_CONTEXT((#19069))
GLOBAL_UNIT_ASSIGNED_CONTEXT((#19091,#19093,#19094))
REPRESENTATION_CONTEXT('','3D')
);
#19083=(
GEOMETRIC_REPRESENTATION_CONTEXT(3)
GLOBAL_UNCERTAINTY_ASSIGNED_CONTEXT((#19070))
GLOBAL_UNIT_ASSIGNED_CONTEXT((#19091,#19093,#19094))
REPRESENTATION_CONTEXT('','3D')
);
#19084=(
GEOMETRIC_REPRESENTATION_CONTEXT(3)
GLOBAL_UNCERTAINTY_ASSIGNED_CONTEXT((#19071))
GLOBAL_UNIT_ASSIGNED_CONTEXT((#19091,#19093,#19094))
REPRESENTATION_CONTEXT('','3D')
);
#19085=(
GEOMETRIC_REPRESENTATION_CONTEXT(3)
GLOBAL_UNCERTAINTY_ASSIGNED_CONTEXT((#19072))
GLOBAL_UNIT_ASSIGNED_CONTEXT((#19091,#19093,#19094))
REPRESENTATION_CONTEXT('','3D')
);
#19086=(
GEOMETRIC_REPRESENTATION_CONTEXT(3)
GLOBAL_UNCERTAINTY_ASSIGNED_CONTEXT((#19073))
GLOBAL_UNIT_ASSIGNED_CONTEXT((#19091,#19093,#19094))
REPRESENTATION_CONTEXT('','3D')
);
#19087=(
GEOMETRIC_REPRESENTATION_CONTEXT(3)
GLOBAL_UNCERTAINTY_ASSIGNED_CONTEXT((#19074))
GLOBAL_UNIT_ASSIGNED_CONTEXT((#19091,#19093,#19094))
REPRESENTATION_CONTEXT('','3D')
);
#19088=(
GEOMETRIC_REPRESENTATION_CONTEXT(3)
GLOBAL_UNCERTAINTY_ASSIGNED_CONTEXT((#19075))
GLOBAL_UNIT_ASSIGNED_CONTEXT((#19091,#19093,#19094))
REPRESENTATION_CONTEXT('','3D')
);
#19089=(
GEOMETRIC_REPRESENTATION_CONTEXT(3)
GLOBAL_UNCERTAINTY_ASSIGNED_CONTEXT((#19076))
GLOBAL_UNIT_ASSIGNED_CONTEXT((#19091,#19093,#19094))
REPRESENTATION_CONTEXT('','3D')
);
#19090=(
GEOMETRIC_REPRESENTATION_CONTEXT(3)
GLOBAL_UNCERTAINTY_ASSIGNED_CONTEXT((#19077))
GLOBAL_UNIT_ASSIGNED_CONTEXT((#19091,#19093,#19094))
REPRESENTATION_CONTEXT('','3D')
);
#19091=(
LENGTH_UNIT()
NAMED_UNIT(*)
SI_UNIT(.CENTI.,.METRE.)
);
#19092=(
LENGTH_UNIT()
NAMED_UNIT(*)
SI_UNIT($,.METRE.)
);
#19093=(
NAMED_UNIT(*)
PLANE_ANGLE_UNIT()
SI_UNIT($,.RADIAN.)
);
#19094=(
NAMED_UNIT(*)
SI_UNIT($,.STERADIAN.)
SOLID_ANGLE_UNIT()
);
#19095=SHAPE_DEFINITION_REPRESENTATION(#19107,#19135);
#19096=SHAPE_DEFINITION_REPRESENTATION(#19108,#19136);
#19097=SHAPE_DEFINITION_REPRESENTATION(#19109,#19137);
#19098=SHAPE_DEFINITION_REPRESENTATION(#19110,#19138);
#19099=SHAPE_DEFINITION_REPRESENTATION(#19111,#19139);
#19100=SHAPE_DEFINITION_REPRESENTATION(#19112,#19140);
#19101=SHAPE_DEFINITION_REPRESENTATION(#19113,#19141);
#19102=SHAPE_DEFINITION_REPRESENTATION(#19114,#19142);
#19103=SHAPE_DEFINITION_REPRESENTATION(#19115,#19143);
#19104=SHAPE_DEFINITION_REPRESENTATION(#19116,#19144);
#19105=SHAPE_DEFINITION_REPRESENTATION(#19117,#19145);
#19106=SHAPE_DEFINITION_REPRESENTATION(#19126,#19146);
#19107=PRODUCT_DEFINITION_SHAPE('',$,#19148);
#19108=PRODUCT_DEFINITION_SHAPE('',$,#19149);
#19109=PRODUCT_DEFINITION_SHAPE('',$,#19150);
#19110=PRODUCT_DEFINITION_SHAPE('',$,#19151);
#19111=PRODUCT_DEFINITION_SHAPE('',$,#19152);
#19112=PRODUCT_DEFINITION_SHAPE('',$,#19153);
#19113=PRODUCT_DEFINITION_SHAPE('',$,#19154);
#19114=PRODUCT_DEFINITION_SHAPE('',$,#19155);
#19115=PRODUCT_DEFINITION_SHAPE('',$,#19156);
#19116=PRODUCT_DEFINITION_SHAPE('',$,#19157);
#19117=PRODUCT_DEFINITION_SHAPE('',$,#19158);
#19118=PRODUCT_DEFINITION_SHAPE($,$,#59);
#19119=PRODUCT_DEFINITION_SHAPE($,$,#60);
#19120=PRODUCT_DEFINITION_SHAPE($,$,#61);
#19121=PRODUCT_DEFINITION_SHAPE($,$,#62);
#19122=PRODUCT_DEFINITION_SHAPE($,$,#63);
#19123=PRODUCT_DEFINITION_SHAPE($,$,#64);
#19124=PRODUCT_DEFINITION_SHAPE($,$,#65);
#19125=PRODUCT_DEFINITION_SHAPE($,$,#66);
#19126=PRODUCT_DEFINITION_SHAPE('',$,#19159);
#19127=PRODUCT_DEFINITION_SHAPE($,$,#67);
#19128=PRODUCT_DEFINITION_SHAPE($,$,#68);
#19129=PRODUCT_DEFINITION_SHAPE($,$,#69);
#19130=PRODUCT_DEFINITION_SHAPE($,$,#70);
#19131=PRODUCT_DEFINITION_SHAPE($,$,#71);
#19132=PRODUCT_DEFINITION_SHAPE($,$,#72);
#19133=PRODUCT_DEFINITION_SHAPE($,$,#73);
#19134=PRODUCT_DEFINITION_SHAPE($,$,#74);
#19135=SHAPE_REPRESENTATION('',(#6941,#7429,#7430,#7431,#7432,#7433,#7434,
#7435,#7436),#19078);
#19136=SHAPE_REPRESENTATION('',(#6942),#19079);
#19137=SHAPE_REPRESENTATION('',(#6980),#19080);
#19138=SHAPE_REPRESENTATION('',(#7011),#19081);
#19139=SHAPE_REPRESENTATION('',(#7029),#19082);
#19140=SHAPE_REPRESENTATION('',(#7040,#7412,#7413,#7414,#7415,#7416,#7417,
#7418,#7419),#19083);
#19141=SHAPE_REPRESENTATION('',(#7041),#19084);
#19142=SHAPE_REPRESENTATION('',(#7143),#19085);
#19143=SHAPE_REPRESENTATION('',(#7251),#19086);
#19144=SHAPE_REPRESENTATION('',(#7304),#19087);
#19145=SHAPE_REPRESENTATION('',(#7386),#19088);
#19146=SHAPE_REPRESENTATION('',(#7420),#19089);
#19147=PRODUCT_DEFINITION_CONTEXT('part definition',#19185,'design');
#19148=PRODUCT_DEFINITION('TOOL-022','TOOL-022',#19160,#19147);
#19149=PRODUCT_DEFINITION('Forged jaw and handle',
'Forged jaw and handle',#19161,#19147);
#19150=PRODUCT_DEFINITION('Moving jaw and handle',
'Moving jaw and handle',#19162,#19147);
#19151=PRODUCT_DEFINITION('Shoulder pivot pin','Shoulder pivot pin',#19163,
#19147);
#19152=PRODUCT_DEFINITION('Pivot retaining ring','Pivot retaining ring',
#19164,#19147);
#19153=PRODUCT_DEFINITION('Grip module 002 style',
'Grip module 002 style',#19165,#19147);
#19154=PRODUCT_DEFINITION('2026-11-10-05-09-19-254',
'Upper structural shell',#19166,#19147);
#19155=PRODUCT_DEFINITION('2026-11-10-05-09-19-258',
'Lower structural shell',#19167,#19147);
#19156=PRODUCT_DEFINITION('2026-11-10-05-09-19-263','Soft grip layer',#19168,
#19147);
#19157=PRODUCT_DEFINITION('2026-11-10-05-09-19-266',
'Socket head cap screw M3x16',#19169,#19147);
#19158=PRODUCT_DEFINITION('2026-11-10-05-09-19-267','Hex nut M3',#19170,
#19147);
#19159=PRODUCT_DEFINITION('Pivot thrust washer','Pivot thrust washer',#19171,
#19147);
#19160=PRODUCT_DEFINITION_FORMATION('',$,#19187);
#19161=PRODUCT_DEFINITION_FORMATION('',$,#19188);
#19162=PRODUCT_DEFINITION_FORMATION('',$,#19189);
#19163=PRODUCT_DEFINITION_FORMATION('',$,#19190);
#19164=PRODUCT_DEFINITION_FORMATION('',$,#19191);
#19165=PRODUCT_DEFINITION_FORMATION('',$,#19192);
#19166=PRODUCT_DEFINITION_FORMATION('',$,#19193);
#19167=PRODUCT_DEFINITION_FORMATION('',$,#19194);
#19168=PRODUCT_DEFINITION_FORMATION('',$,#19195);
#19169=PRODUCT_DEFINITION_FORMATION('',$,#19196);
#19170=PRODUCT_DEFINITION_FORMATION('',$,#19197);
#19171=PRODUCT_DEFINITION_FORMATION('',$,#19198);
#19172=PRODUCT_RELATED_PRODUCT_CATEGORY('TOOL-022','TOOL-022',(#19187));
#19173=PRODUCT_RELATED_PRODUCT_CATEGORY('Forged jaw and handle',
'Forged jaw and handle',(#19188));
#19174=PRODUCT_RELATED_PRODUCT_CATEGORY('Moving jaw and handle',
'Moving jaw and handle',(#19189));
#19175=PRODUCT_RELATED_PRODUCT_CATEGORY('Shoulder pivot pin',
'Shoulder pivot pin',(#19190));
#19176=PRODUCT_RELATED_PRODUCT_CATEGORY('Pivot retaining ring',
'Pivot retaining ring',(#19191));
#19177=PRODUCT_RELATED_PRODUCT_CATEGORY('Grip module 002 style',
'Grip module 002 style',(#19192));
#19178=PRODUCT_RELATED_PRODUCT_CATEGORY('Upper structural shell',
'Upper structural shell',(#19193));
#19179=PRODUCT_RELATED_PRODUCT_CATEGORY('Lower structural shell',
'Lower structural shell',(#19194));
#19180=PRODUCT_RELATED_PRODUCT_CATEGORY('Soft grip layer',
'Soft grip layer',(#19195));
#19181=PRODUCT_RELATED_PRODUCT_CATEGORY('Socket head cap screw M3x16',
'Socket head cap screw M3x16',(#19196));
#19182=PRODUCT_RELATED_PRODUCT_CATEGORY('Hex nut M3','Hex nut M3',(#19197));
#19183=PRODUCT_RELATED_PRODUCT_CATEGORY('Pivot thrust washer',
'Pivot thrust washer',(#19198));
#19184=APPLICATION_PROTOCOL_DEFINITION('international standard',
'automotive_design',2009,#19185);
#19185=APPLICATION_CONTEXT(
'Core Data for Automotive Mechanical Design Process');
#19186=PRODUCT_CONTEXT('part definition',#19185,'mechanical');
#19187=PRODUCT('TOOL-022','TOOL-022',$,(#19186));
#19188=PRODUCT('Forged jaw and handle','Forged jaw and handle',$,(#19186));
#19189=PRODUCT('Moving jaw and handle','Moving jaw and handle',$,(#19186));
#19190=PRODUCT('Shoulder pivot pin','Shoulder pivot pin',$,(#19186));
#19191=PRODUCT('Pivot retaining ring','Pivot retaining ring',$,(#19186));
#19192=PRODUCT('Grip module 002 style','Grip module 002 style',$,(#19186));
#19193=PRODUCT('2026-11-10-05-09-19-254','Upper structural shell',$,(#19186));
#19194=PRODUCT('2026-11-10-05-09-19-258','Lower structural shell',$,(#19186));
#19195=PRODUCT('2026-11-10-05-09-19-263','Soft grip layer',$,(#19186));
#19196=PRODUCT('2026-11-10-05-09-19-266','Socket head cap screw M3x16',
$,(#19186));
#19197=PRODUCT('2026-11-10-05-09-19-267','Hex nut M3',$,(#19186));
#19198=PRODUCT('Pivot thrust washer','Pivot thrust washer',$,(#19186));
#19199=PRESENTATION_STYLE_ASSIGNMENT((#19207));
#19200=PRESENTATION_STYLE_ASSIGNMENT((#19208));
#19201=PRESENTATION_STYLE_ASSIGNMENT((#19209));
#19202=PRESENTATION_STYLE_ASSIGNMENT((#19210));
#19203=PRESENTATION_STYLE_ASSIGNMENT((#19211));
#19204=PRESENTATION_STYLE_ASSIGNMENT((#19212));
#19205=PRESENTATION_STYLE_ASSIGNMENT((#19213));
#19206=PRESENTATION_STYLE_ASSIGNMENT((#19214));
#19207=SURFACE_STYLE_USAGE(.BOTH.,#19215);
#19208=SURFACE_STYLE_USAGE(.BOTH.,#19216);
#19209=SURFACE_STYLE_USAGE(.BOTH.,#19217);
#19210=SURFACE_STYLE_USAGE(.BOTH.,#19218);
#19211=SURFACE_STYLE_USAGE(.BOTH.,#19219);
#19212=SURFACE_STYLE_USAGE(.BOTH.,#19220);
#19213=SURFACE_STYLE_USAGE(.BOTH.,#19221);
#19214=SURFACE_STYLE_USAGE(.BOTH.,#19222);
#19215=SURFACE_SIDE_STYLE('',(#19223));
#19216=SURFACE_SIDE_STYLE('',(#19224));
#19217=SURFACE_SIDE_STYLE('',(#19225));
#19218=SURFACE_SIDE_STYLE('',(#19226));
#19219=SURFACE_SIDE_STYLE('',(#19227));
#19220=SURFACE_SIDE_STYLE('',(#19228));
#19221=SURFACE_SIDE_STYLE('',(#19229));
#19222=SURFACE_SIDE_STYLE('',(#19230));
#19223=SURFACE_STYLE_FILL_AREA(#19231);
#19224=SURFACE_STYLE_FILL_AREA(#19232);
#19225=SURFACE_STYLE_FILL_AREA(#19233);
#19226=SURFACE_STYLE_FILL_AREA(#19234);
#19227=SURFACE_STYLE_FILL_AREA(#19235);
#19228=SURFACE_STYLE_FILL_AREA(#19236);
#19229=SURFACE_STYLE_FILL_AREA(#19237);
#19230=SURFACE_STYLE_FILL_AREA(#19238);
#19231=FILL_AREA_STYLE('Steel - Satin',(#19239));
#19232=FILL_AREA_STYLE('Tool steel gray',(#19240));
#19233=FILL_AREA_STYLE('Pivot dark gray',(#19241));
#19234=FILL_AREA_STYLE('Dark gray',(#19242));
#19235=FILL_AREA_STYLE('Structural dark blue',(#19243));
#19236=FILL_AREA_STYLE('Sky blue soft grip',(#19244));
#19237=FILL_AREA_STYLE('Fastener gray',(#19245));
#19238=FILL_AREA_STYLE('Washer gray',(#19246));
#19239=FILL_AREA_STYLE_COLOUR('Steel - Satin',#19247);
#19240=FILL_AREA_STYLE_COLOUR('Tool steel gray',#19248);
#19241=FILL_AREA_STYLE_COLOUR('Pivot dark gray',#19249);
#19242=FILL_AREA_STYLE_COLOUR('Dark gray',#19250);
#19243=FILL_AREA_STYLE_COLOUR('Structural dark blue',#19251);
#19244=FILL_AREA_STYLE_COLOUR('Sky blue soft grip',#19252);
#19245=FILL_AREA_STYLE_COLOUR('Fastener gray',#19253);
#19246=FILL_AREA_STYLE_COLOUR('Washer gray',#19254);
#19247=COLOUR_RGB('Steel - Satin',0.627450980392157,0.627450980392157,0.627450980392157);
#19248=COLOUR_RGB('Tool steel gray',0.607843137254902,0.643137254901961,
0.698039215686274);
#19249=COLOUR_RGB('Pivot dark gray',0.27843137254902,0.309803921568627,
0.352941176470588);
#19250=COLOUR_RGB('Dark gray',0.250980392156863,0.282352941176471,0.32156862745098);
#19251=COLOUR_RGB('Structural dark blue',0.0901960784313725,0.270588235294118,
0.513725490196078);
#19252=COLOUR_RGB('Sky blue soft grip',0.27843137254902,0.309803921568627,
0.352941176470588);
#19253=COLOUR_RGB('Fastener gray',0.607843137254902,0.643137254901961,0.698039215686274);
#19254=COLOUR_RGB('Washer gray',0.725490196078431,0.752941176470588,0.792156862745098);
ENDSEC;
END-ISO-10303-21;
